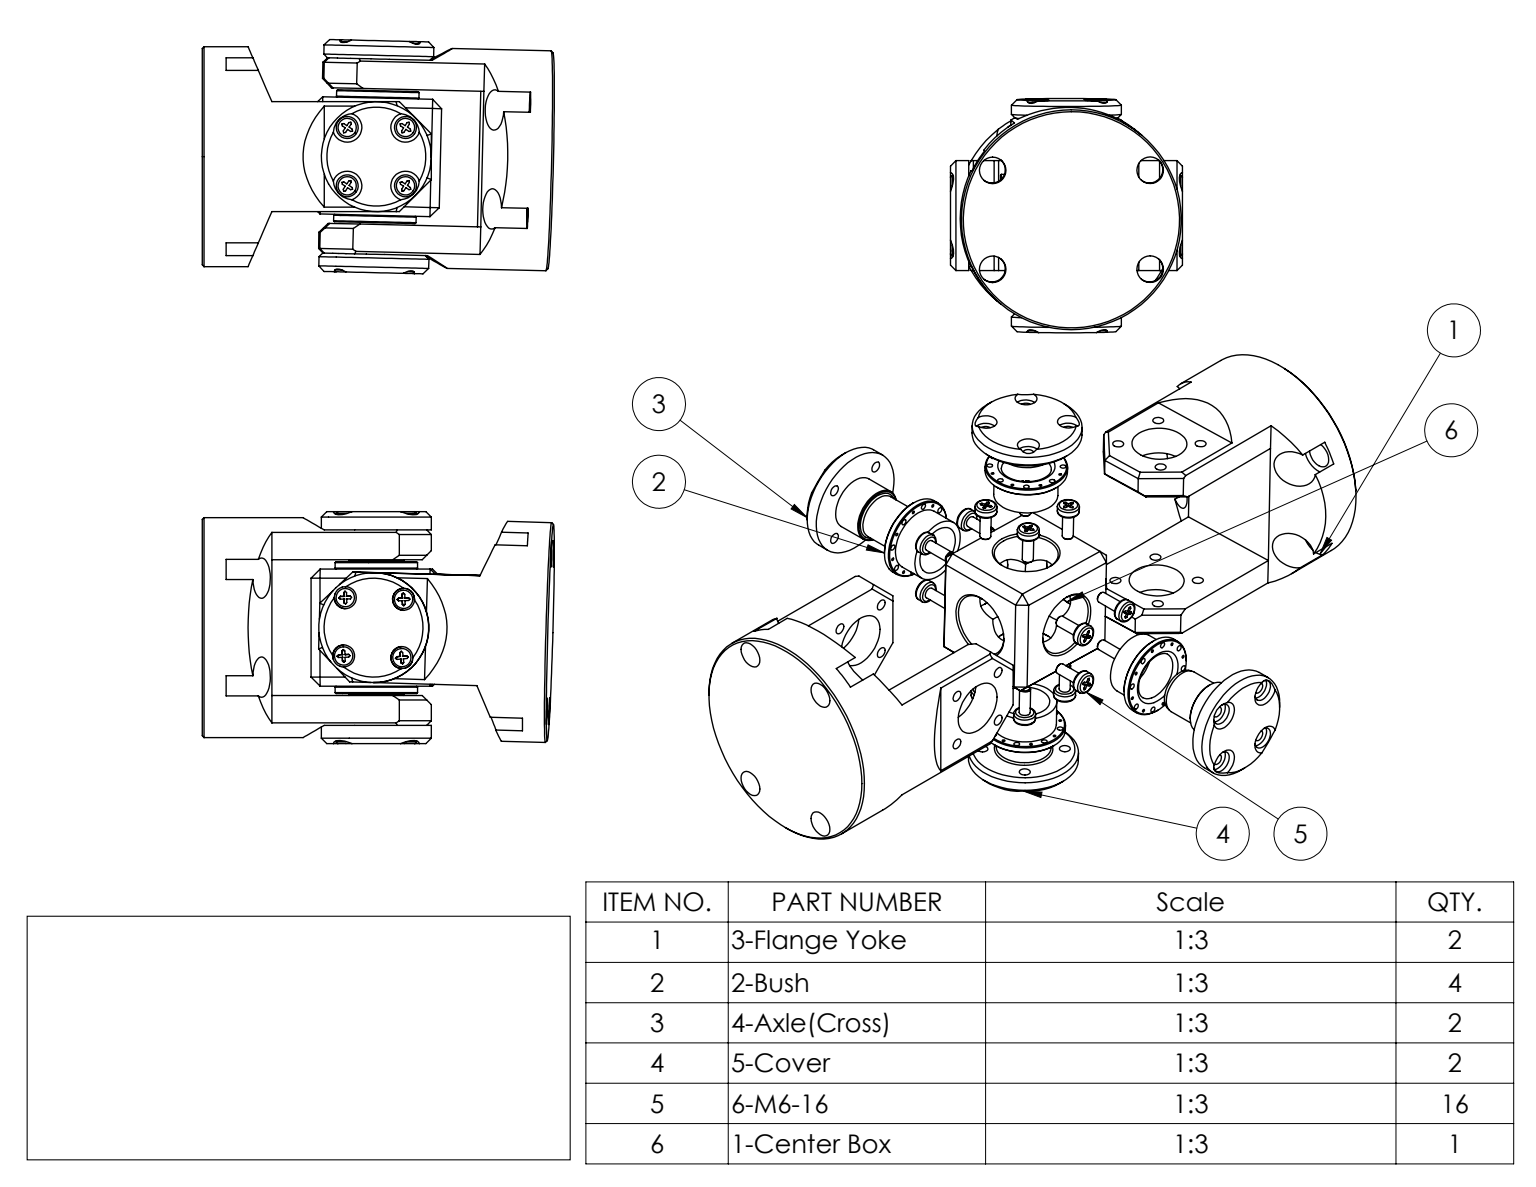
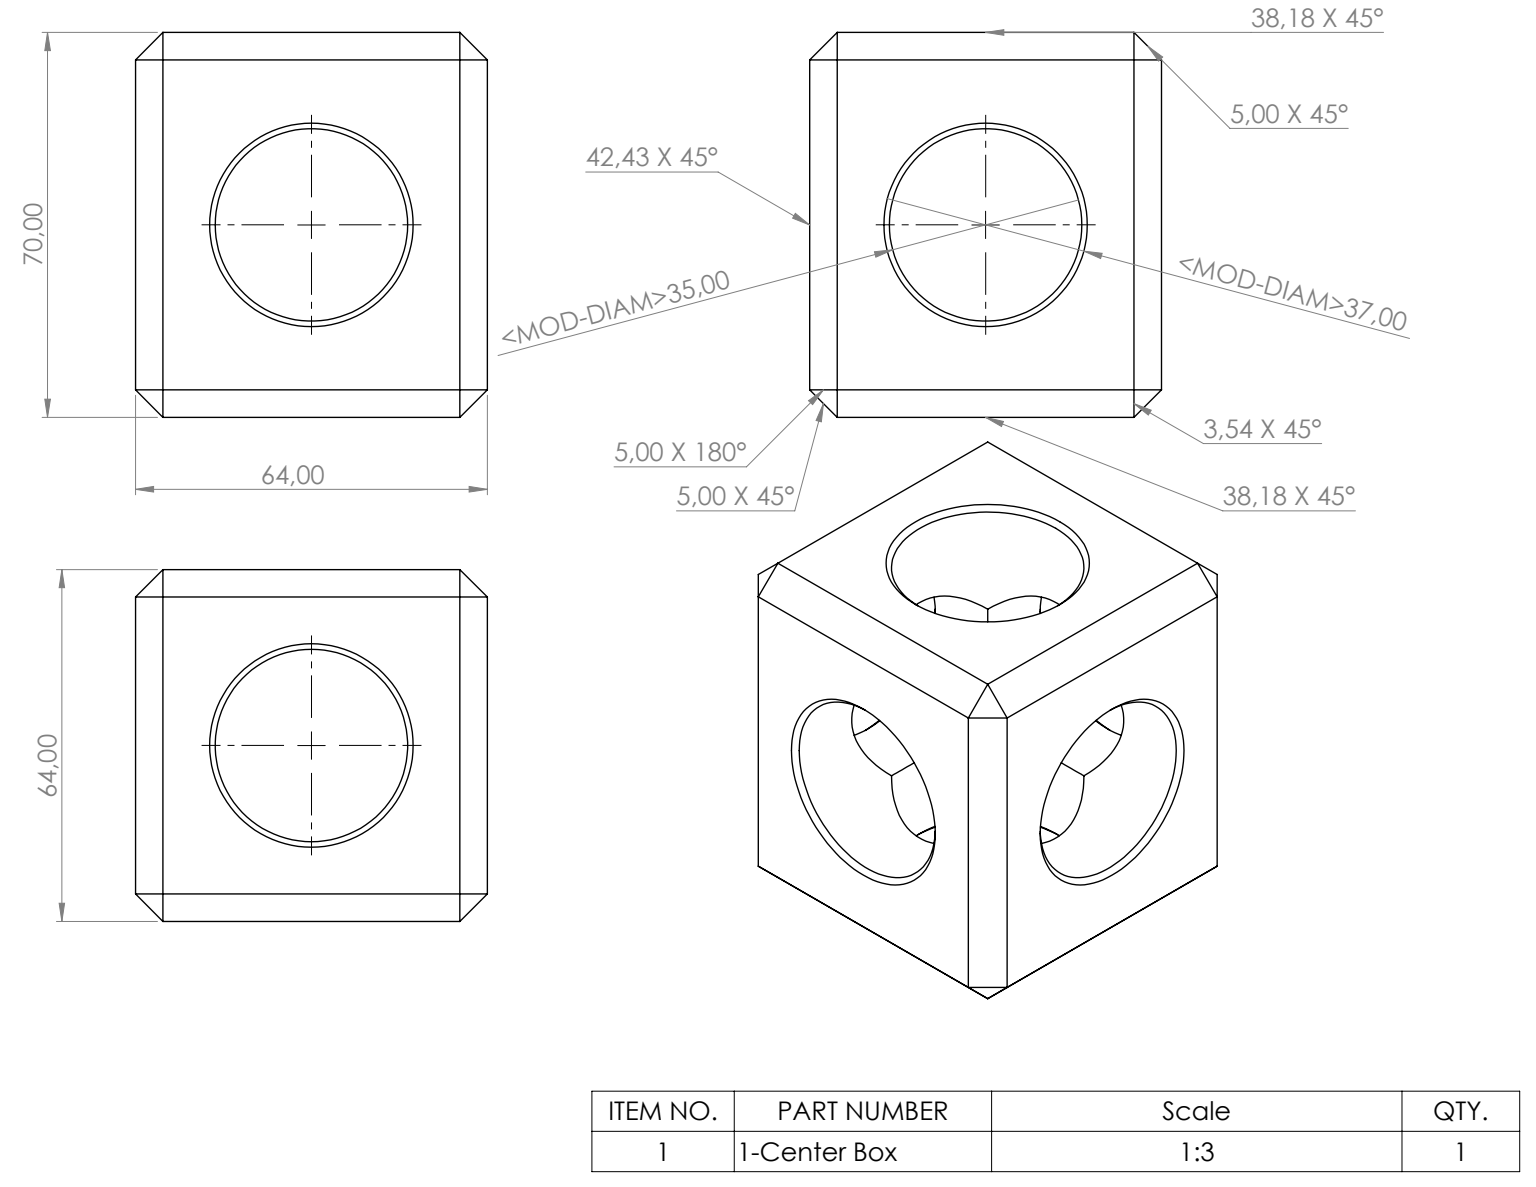
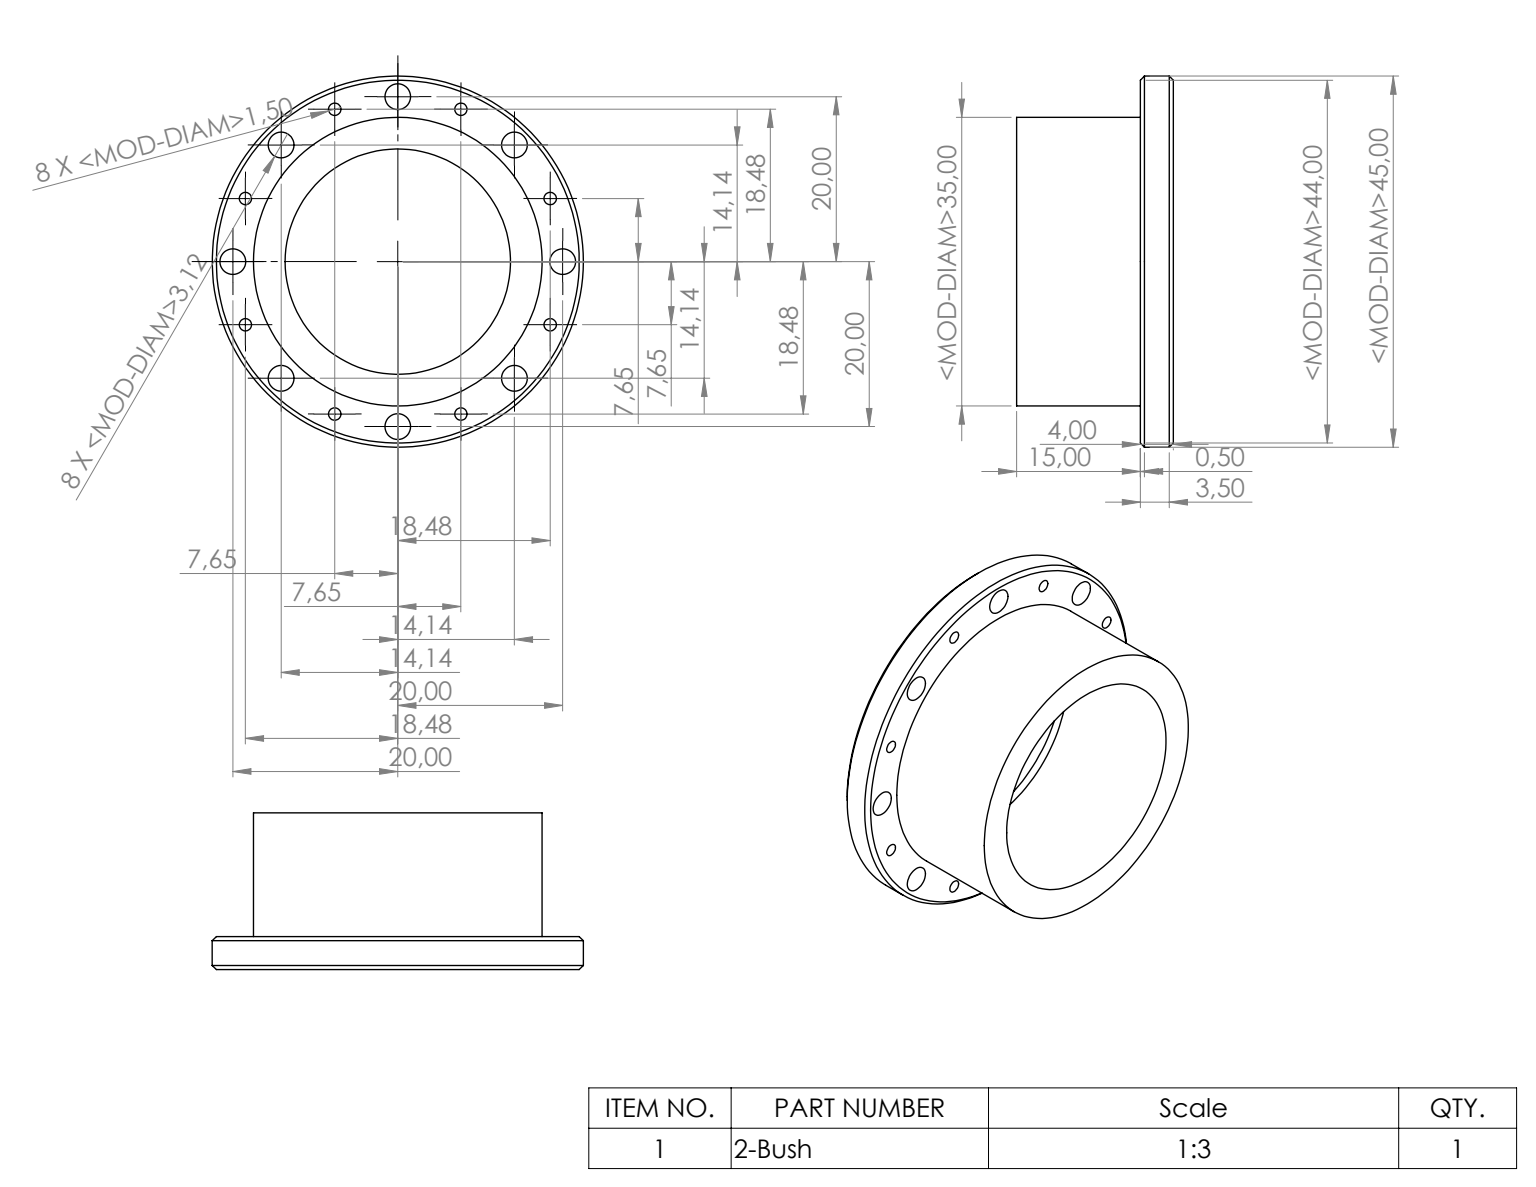
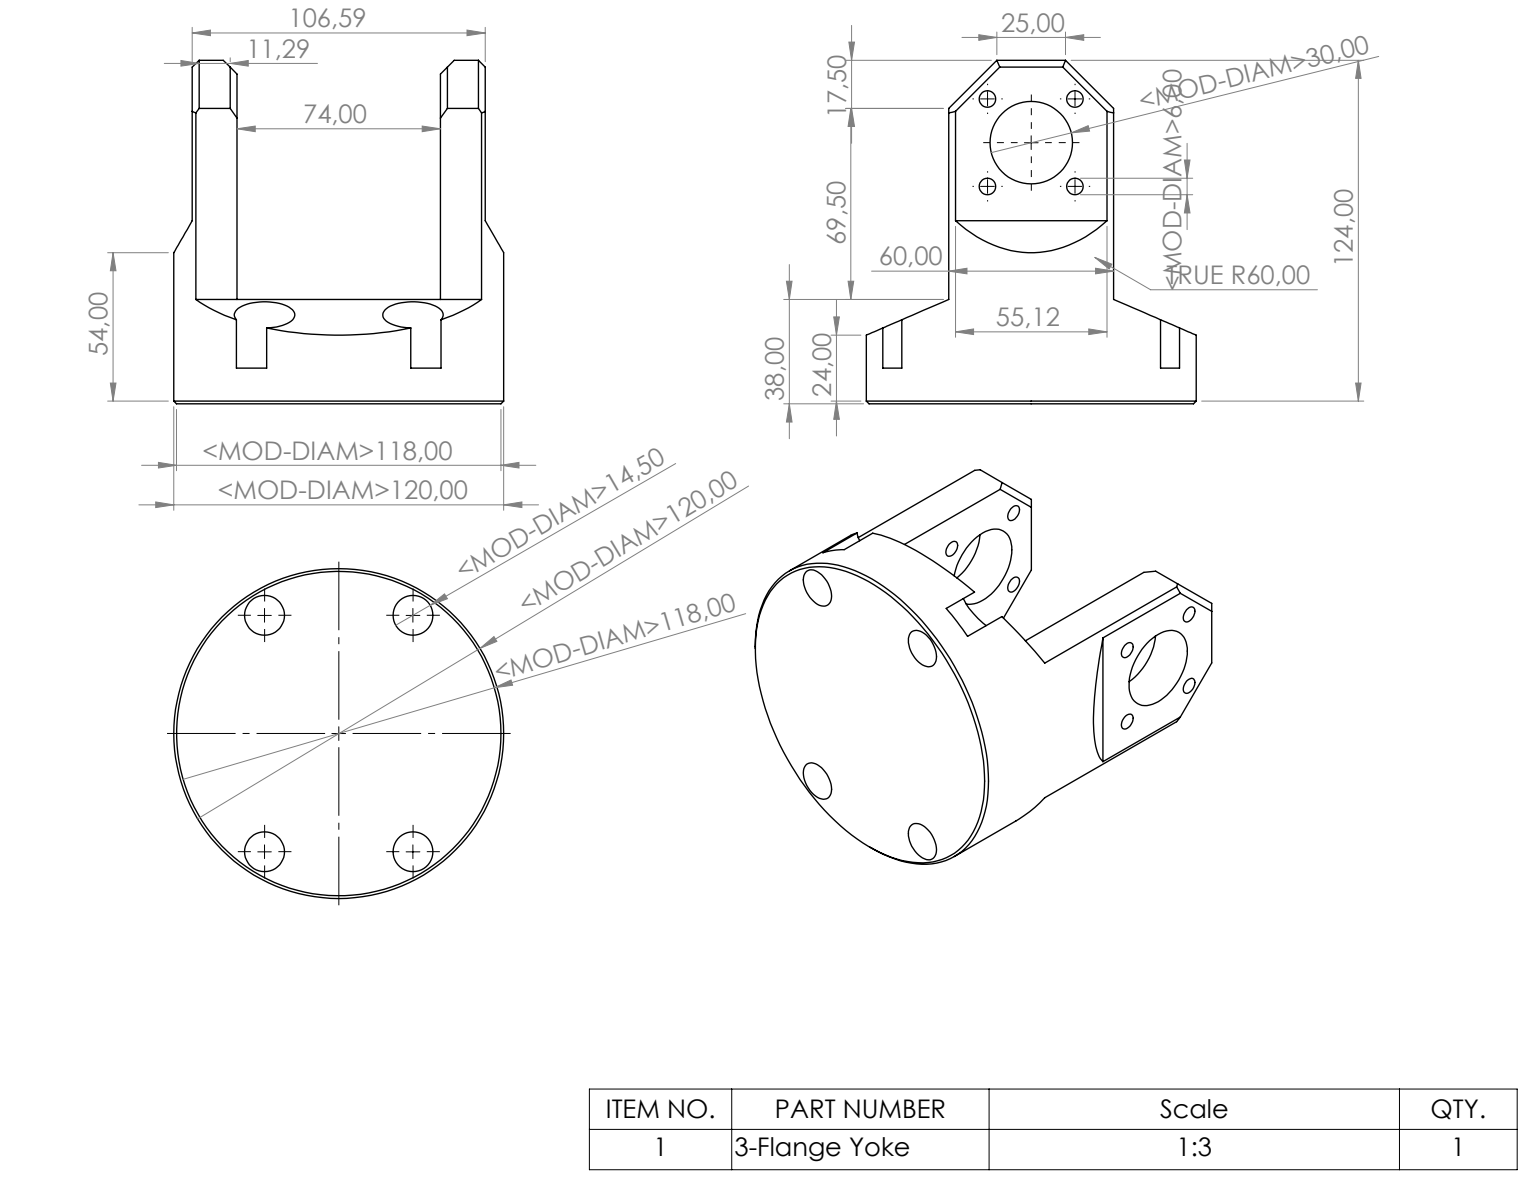
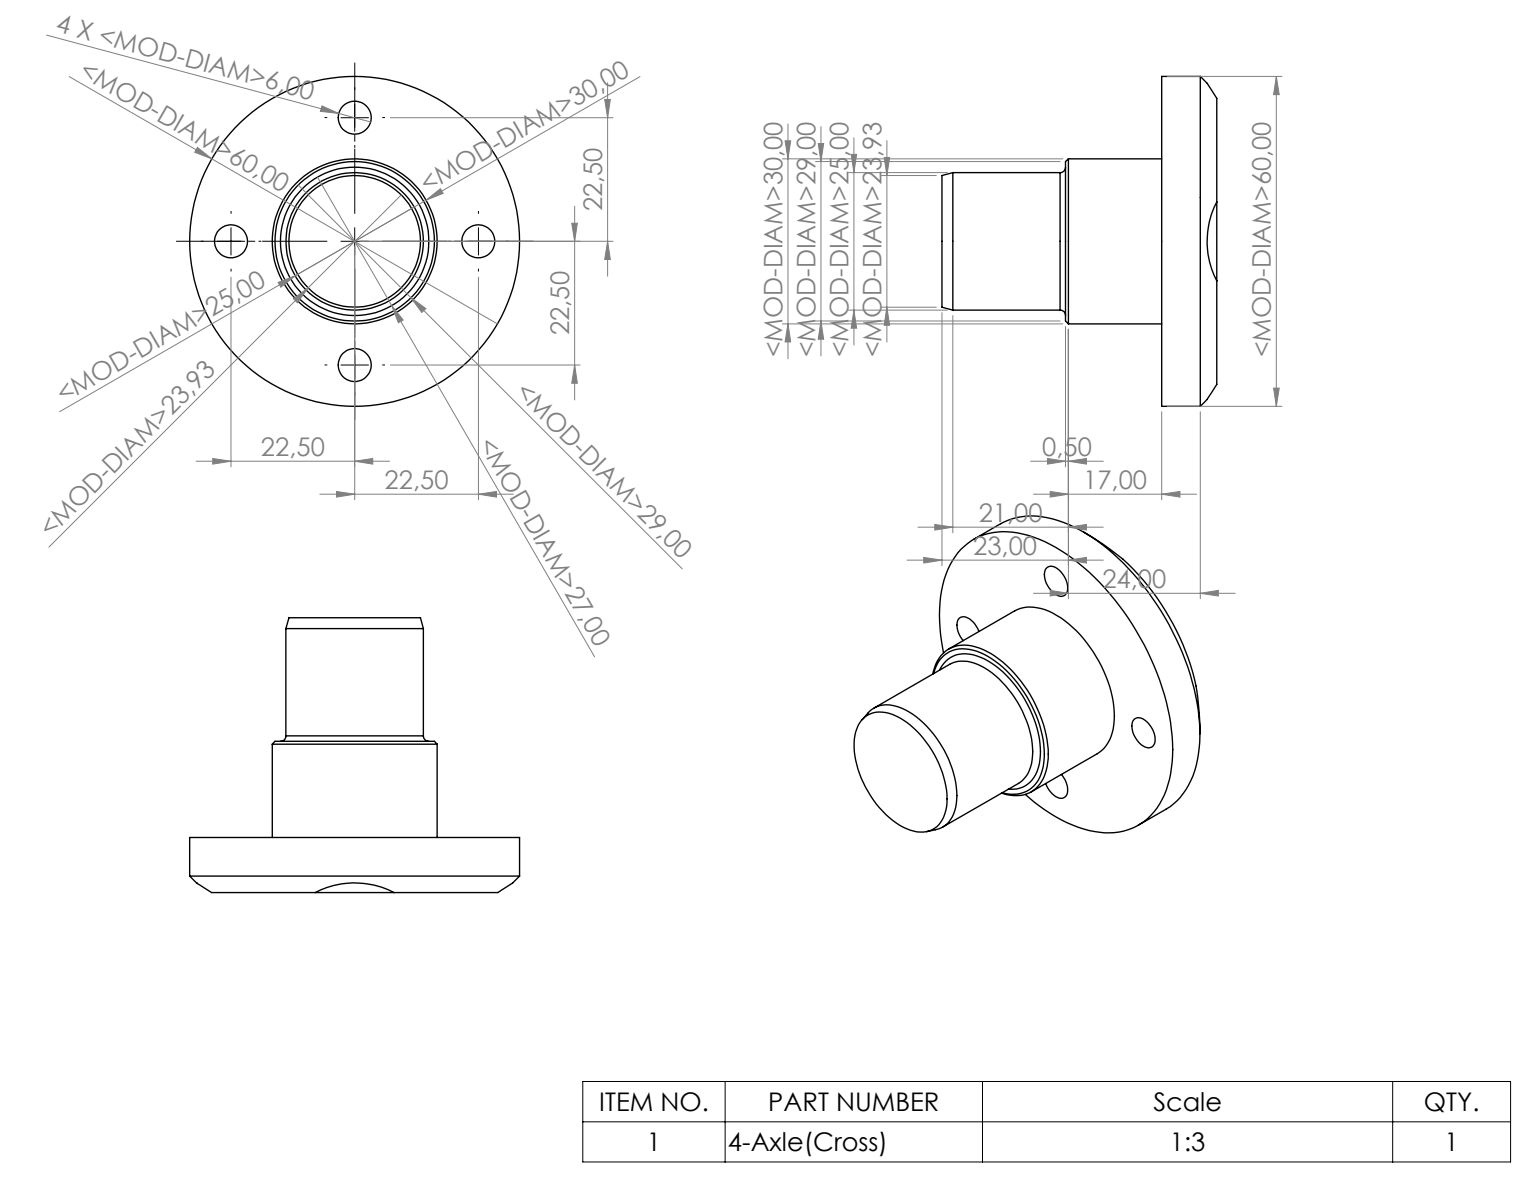
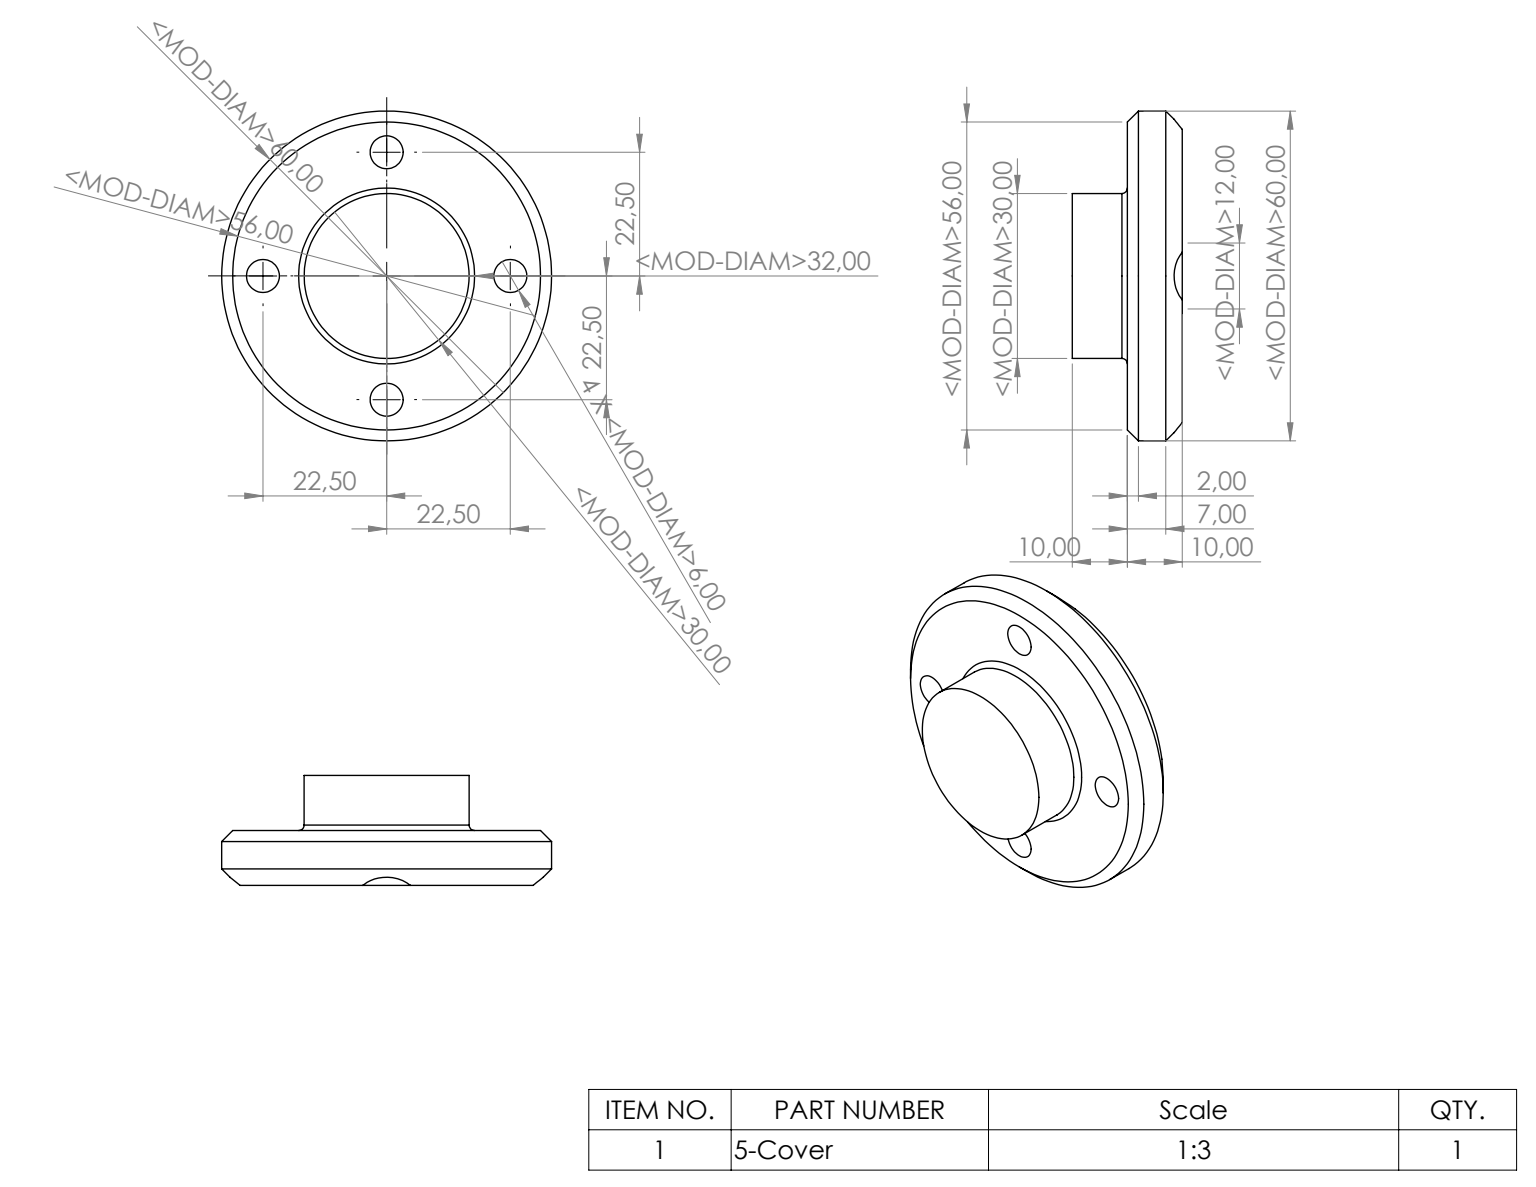
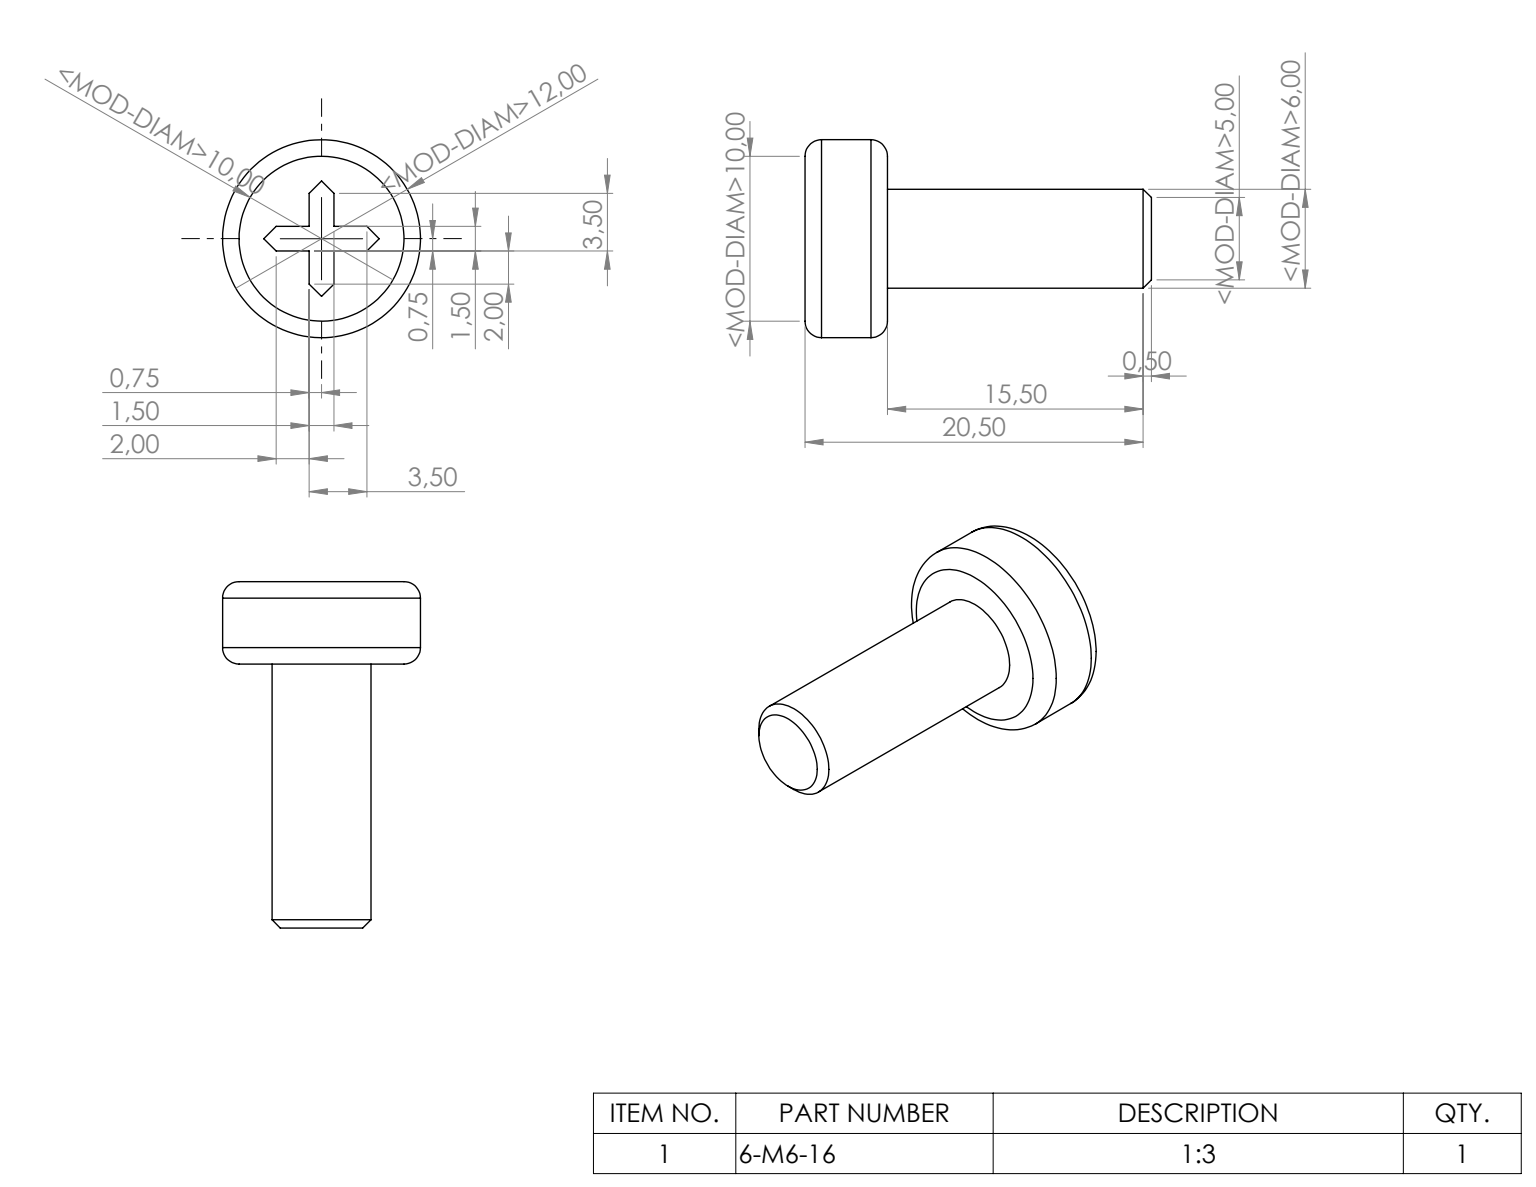
ISO-10303-21;
HEADER;
FILE_DESCRIPTION (('STEP AP214'),
    '1' );
FILE_NAME ('MAT-017',
    '2026-10-28T16:50:19',
    ( '' ),
    ( '' ),
    'SwSTEP 2.0',
    'SolidWorks 2024',
    '' );
FILE_SCHEMA (( 'AUTOMOTIVE_DESIGN' ));
ENDSEC;

DATA;
#1 = DIRECTION ( 'NONE',  ( -0.7071067811865456854, 9.059701919605289623E-16, -0.7071067811865493491 ) ) ;
#2 = FACE_BOUND ( 'NONE', #8236, .T. ) ;
#3 = FACE_OUTER_BOUND ( 'NONE', #2882, .T. ) ;
#4 = ORIENTED_EDGE ( 'NONE', *, *, #2008, .F. ) ;
#5 = EDGE_LOOP ( 'NONE', ( #4798, #3652 ) ) ;
#6 = EDGE_CURVE ( 'NONE', #2372, #8340, #1987, .T. ) ;
#7 = ORIENTED_EDGE ( 'NONE', *, *, #437, .T. ) ;
#8 = DIRECTION ( 'NONE',  ( -2.852901704589927581E-15, -0.02376617340079590149, -0.9997175446104182850 ) ) ;
#9 = ORIENTED_EDGE ( 'NONE', *, *, #306, .F. ) ;
#10 = CARTESIAN_POINT ( 'NONE',  ( -22.50000000000000000, -7.855833012397050680E-14, 5.000000000000000000 ) ) ;
#11 = LINE ( 'NONE', #2843, #879 ) ;
#12 = DIRECTION ( 'NONE',  ( 0.000000000000000000, 0.000000000000000000, -1.000000000000000000 ) ) ;
#13 = CARTESIAN_POINT ( 'NONE',  ( 15.00000000000000000, 1.836970198721029589E-15, 11.00000000000000000 ) ) ;
#14 = CARTESIAN_POINT ( 'NONE',  ( 26.21170834203230982, 53.97171801779368394, -2.612255525622733554 ) ) ;
#15 = EDGE_CURVE ( 'NONE', #5505, #2772, #7117, .T. ) ;
#16 = LINE ( 'NONE', #2270, #110 ) ;
#17 = CIRCLE ( 'NONE', #5073, 3.000000000000000444 ) ;
#18 = VERTEX_POINT ( 'NONE', #6645 ) ;
#19 = EDGE_CURVE ( 'NONE', #8372, #438, #65, .T. ) ;
#20 = DIRECTION ( 'NONE',  ( 0.000000000000000000, 0.000000000000000000, -1.000000000000000000 ) ) ;
#21 = EDGE_CURVE ( 'NONE', #6915, #8464, #3515, .T. ) ;
#22 = EDGE_CURVE ( 'NONE', #2924, #3020, #3177, .T. ) ;
#23 = VERTEX_POINT ( 'NONE', #8844 ) ;
#24 = DIRECTION ( 'NONE',  ( 0.7071067811865494601, 0.7071067811865455743, 0.000000000000000000 ) ) ;
#25 = DIRECTION ( 'NONE',  ( -1.000000000000000000, 0.000000000000000000, 0.000000000000000000 ) ) ;
#26 = VECTOR ( 'NONE', #5373, 1000.000000000000000 ) ;
#27 = LINE ( 'NONE', #8090, #5201 ) ;
#28 = DIRECTION ( 'NONE',  ( -1.000000000000000000, -0.000000000000000000, -0.000000000000000000 ) ) ;
#29 = PRODUCT_DEFINITION_SHAPE ( 'NONE', 'NONE',  #9491 ) ;
#30 = ORIENTED_EDGE ( 'NONE', *, *, #4937, .F. ) ;
#31 = VERTEX_POINT ( 'NONE', #8796 ) ;
#32 = CARTESIAN_POINT ( 'NONE',  ( 3.791949971500756078, 27.16611547376996683, 0.4273392542514659609 ) ) ;
#33 = ORIENTED_EDGE ( 'NONE', *, *, #310, .F. ) ;
#34 = DIRECTION ( 'NONE',  ( 0.000000000000000000, 0.000000000000000000, 1.000000000000000000 ) ) ;
#35 = CARTESIAN_POINT ( 'NONE',  ( 28.50000000000000355, 7.347880794884122694E-16, 5.000000000000000000 ) ) ;
#36 =( BOUNDED_CURVE ( )  B_SPLINE_CURVE ( 3, ( #9430, #2857, #1405, #8718 ),
 .UNSPECIFIED., .F., .F. ) 
 B_SPLINE_CURVE_WITH_KNOTS ( ( 4, 4 ),
 ( 0.6692669939101983934, 1.047197551196597853 ),
 .UNSPECIFIED. ) 
 CURVE ( )  GEOMETRIC_REPRESENTATION_ITEM ( )  RATIONAL_B_SPLINE_CURVE ( ( 1.000000000000000000, 0.9881327504826167285, 0.9881327504826167285, 1.000000000000000000 ) ) 
 REPRESENTATION_ITEM ( '' )  );
#37 = EDGE_CURVE ( 'NONE', #4781, #2523, #3325, .T. ) ;
#38 = CARTESIAN_POINT ( 'NONE',  ( 0.7500000000000000000, 2.749999999999995559, 0.000000000000000000 ) ) ;
#39 = AXIS2_PLACEMENT_3D ( 'NONE', #7750, #9043, #8374 ) ;
#40 = CARTESIAN_POINT ( 'NONE',  ( 29.50000000000000711, -29.99999999999996447, 2.500000000000015543 ) ) ;
#41 = LINE ( 'NONE', #8503, #1449 ) ;
#42 = ADVANCED_FACE ( 'NONE', ( #1448 ), #3565, .F. ) ;
#43 = FACE_OUTER_BOUND ( 'NONE', #6081, .T. ) ;
#44 = CARTESIAN_POINT ( 'NONE',  ( 0.000000000000000000, 0.000000000000000000, 0.000000000000000000 ) ) ;
#45 = ORIENTED_EDGE ( 'NONE', *, *, #8118, .F. ) ;
#46 = ORIENTED_EDGE ( 'NONE', *, *, #483, .F. ) ;
#47 = CARTESIAN_POINT ( 'NONE',  ( -53.29490495164537833, 15.90990257669733943, -54.09009742330271564 ) ) ;
#48 = VECTOR ( 'NONE', #5303, 999.9999999999998863 ) ;
#49 = CARTESIAN_POINT ( 'NONE',  ( 34.25000000000000000, -43.00000000000000000, -25.00000000000000000 ) ) ;
#50 = FACE_OUTER_BOUND ( 'NONE', #5817, .T. ) ;
#51 = DIRECTION ( 'NONE',  ( 0.000000000000000000, 0.000000000000000000, 1.000000000000000000 ) ) ;
#52 = ORIENTED_EDGE ( 'NONE', *, *, #8438, .F. ) ;
#53 = EDGE_LOOP ( 'NONE', ( #8094, #7825 ) ) ;
#54 = CARTESIAN_POINT ( 'NONE',  ( -56.07586385285965491, 64.54333883338065903, 59.86606487507440022 ) ) ;
#55 = VERTEX_POINT ( 'NONE', #1398 ) ;
#56 = EDGE_CURVE ( 'NONE', #523, #4316, #9131, .T. ) ;
#57 = CARTESIAN_POINT ( 'NONE',  ( 29.50000000000000711, -32.49999999999997868, 58.99999999999997158 ) ) ;
#58 = DIRECTION ( 'NONE',  ( -1.000000000000000000, 0.000000000000000000, 0.000000000000000000 ) ) ;
#59 = AXIS2_PLACEMENT_3D ( 'NONE', #1262, #1856, #6375 ) ;
#60 = ADVANCED_FACE ( 'NONE', ( #7941 ), #7013, .F. ) ;
#61 = DIRECTION ( 'NONE',  ( 1.000000000000000000, 0.000000000000000000, 0.000000000000000000 ) ) ;
#62 = CARTESIAN_POINT ( 'NONE',  ( -53.29490495164537833, 15.90990257669733943, -85.90990257669729147 ) ) ;
#63 = CARTESIAN_POINT ( 'NONE',  ( -53.29490495164537833, 15.90990257669733943, -51.09009742330271564 ) ) ;
#64 = EDGE_LOOP ( 'NONE', ( #9455, #3764, #9081, #6496 ) ) ;
#65 = LINE ( 'NONE', #2077, #6706 ) ;
#66 = ORIENTED_EDGE ( 'NONE', *, *, #5730, .F. ) ;
#67 = FACE_OUTER_BOUND ( 'NONE', #9174, .T. ) ;
#68 = CYLINDRICAL_SURFACE ( 'NONE', #4244, 3.000000000000000000 ) ;
#69 = LINE ( 'NONE', #4584, #4436 ) ;
#70 = AXIS2_PLACEMENT_3D ( 'NONE', #3786, #2250, #5184 ) ;
#71 = CARTESIAN_POINT ( 'NONE',  ( 53.29490495164537833, -30.00000000000000000, -97.50000000000002842 ) ) ;
#72 = TOROIDAL_SURFACE ( 'NONE', #5447, 15.66147716702868209, 2.000000000000000000 ) ;
#73 = ORIENTED_EDGE ( 'NONE', *, *, #437, .F. ) ;
#74 = ORIENTED_EDGE ( 'NONE', *, *, #37, .F. ) ;
#75 = VERTEX_POINT ( 'NONE', #1302 ) ;
#76 = FACE_OUTER_BOUND ( 'NONE', #1771, .T. ) ;
#77 = CARTESIAN_POINT ( 'NONE',  ( -4.703319286132082055, 17.49999999999999645, 14.50000000000000178 ) ) ;
#78 = ADVANCED_FACE ( 'NONE', ( #8660 ), #4237, .F. ) ;
#79 = DIRECTION ( 'NONE',  ( 1.000000000000000000, 0.000000000000000000, 0.000000000000000000 ) ) ;
#80 = AXIS2_PLACEMENT_3D ( 'NONE', #2507, #6973, #1060 ) ;
#81 = DIRECTION ( 'NONE',  ( 0.000000000000000000, 0.000000000000000000, -1.000000000000000000 ) ) ;
#82 = DIRECTION ( 'NONE',  ( -1.000000000000000000, 0.000000000000000000, 0.000000000000000000 ) ) ;
#83 = DIRECTION ( 'NONE',  ( 1.224646799147353207E-16, 1.000000000000000000, -0.000000000000000000 ) ) ;
#84 = DIRECTION ( 'NONE',  ( -1.000000000000000000, -0.000000000000000000, -0.000000000000000000 ) ) ;
#85 = VERTEX_POINT ( 'NONE', #733 ) ;
#86 = EDGE_LOOP ( 'NONE', ( #7800, #8743 ) ) ;
#87 = CARTESIAN_POINT ( 'NONE',  ( -19.50000000000000355, 3.673940397442054445E-16, 5.000000000000000000 ) ) ;
#88 = EDGE_LOOP ( 'NONE', ( #1645, #1926, #910, #5468 ) ) ;
#89 = DIRECTION ( 'NONE',  ( 1.000000000000000000, -0.000000000000000000, -0.000000000000000000 ) ) ;
#90 = CARTESIAN_POINT ( 'NONE',  ( 6.702350214711367826, 26.42345776824586423, 0.2543657081580636414 ) ) ;
#91 = DIRECTION ( 'NONE',  ( -0.000000000000000000, -1.000000000000000000, -0.000000000000000000 ) ) ;
#92 = UNCERTAINTY_MEASURE_WITH_UNIT (LENGTH_MEASURE( 1.000000000000000082E-05 ), #7663, 'distance_accuracy_value', 'NONE');
#93 = CARTESIAN_POINT ( 'NONE',  ( 5.000000000000000000, 14.14213562373112154, -14.14213562373077870 ) ) ;
#94 = VECTOR ( 'NONE', #809, 1000.000000000000000 ) ;
#95 = VERTEX_POINT ( 'NONE', #8709 ) ;
#96 = ORIENTED_EDGE ( 'NONE', *, *, #7565, .T. ) ;
#97 = DIRECTION ( 'NONE',  ( 1.000000000000000222, -1.235987831730286119E-16, -8.658028549763971743E-17 ) ) ;
#98 = CARTESIAN_POINT ( 'NONE',  ( 37.00000000000000000, -30.00000000000000000, -95.00000000000000000 ) ) ;
#99 = LINE ( 'NONE', #8746, #418 ) ;
#100 = AXIS2_PLACEMENT_3D ( 'NONE', #6905, #316, #3150 ) ;
#101 = CARTESIAN_POINT ( 'NONE',  ( 0.000000000000000000, 0.000000000000000000, 11.99999999999999645 ) ) ;
#102 = DIRECTION ( 'NONE',  ( -1.000000000000000000, 0.000000000000000000, 0.000000000000000000 ) ) ;
#103 = DIRECTION ( 'NONE',  ( -0.000000000000000000, 0.7071067811865473507, 0.7071067811865477948 ) ) ;
#104 = EDGE_CURVE ( 'NONE', #1161, #4913, #2730, .T. ) ;
#105 = CARTESIAN_POINT ( 'NONE',  ( 4.000000000000000000, 20.00000000000120437, 1.559999999999680531 ) ) ;
#106 = VERTEX_POINT ( 'NONE', #5874 ) ;
#107 = AXIS2_PLACEMENT_3D ( 'NONE', #3229, #1109, #5357 ) ;
#108 = FILL_AREA_STYLE ('',( #7504 ) ) ;
#109 = EDGE_LOOP ( 'NONE', ( #8068, #7356, #2708, #2295 ) ) ;
#110 = VECTOR ( 'NONE', #4520, 1000.000000000000000 ) ;
#111 = CARTESIAN_POINT ( 'NONE',  ( 19.62310601229373930, -19.62310601229373930, 26.87436867076458924 ) ) ;
#112 = EDGE_CURVE ( 'NONE', #6044, #3779, #6462, .T. ) ;
#113 = CARTESIAN_POINT ( 'NONE',  ( 0.000000000000000000, 0.000000000000000000, 0.000000000000000000 ) ) ;
#114 = AXIS2_PLACEMENT_3D ( 'NONE', #1241, #6492, #8505 ) ;
#115 = CIRCLE ( 'NONE', #3792, 1.559999999998939346 ) ;
#116 = CARTESIAN_POINT ( 'NONE',  ( 37.00000000000000000, -15.90990257669733943, -88.90990257669730568 ) ) ;
#117 = AXIS2_PLACEMENT_3D ( 'NONE', #9182, #529, #8560 ) ;
#118 = CARTESIAN_POINT ( 'NONE',  ( -28.50000000000000355, 0.000000000000000000, 5.000000000000000000 ) ) ;
#119 = VECTOR ( 'NONE', #1429, 1000.000000000000114 ) ;
#120 = ORIENTED_EDGE ( 'NONE', *, *, #516, .T. ) ;
#121 = EDGE_LOOP ( 'NONE', ( #3677, #5526, #8764, #3879, #8157 ) ) ;
#122 = AXIS2_PLACEMENT_3D ( 'NONE', #7775, #7822, #1915 ) ;
#123 = ORIENTED_EDGE ( 'NONE', *, *, #4714, .F. ) ;
#124 = ORIENTED_EDGE ( 'NONE', *, *, #9169, .F. ) ;
#125 = ADVANCED_FACE ( 'NONE', ( #5828 ), #4338, .F. ) ;
#126 = AXIS2_PLACEMENT_3D ( 'NONE', #8460, #4038, #6303 ) ;
#127 = CARTESIAN_POINT ( 'NONE',  ( 37.00000000000000000, 30.00000000000000000, -78.96446609406729067 ) ) ;
#128 = DIRECTION ( 'NONE',  ( 0.000000000000000000, 0.000000000000000000, 1.000000000000000000 ) ) ;
#129 = CYLINDRICAL_SURFACE ( 'NONE', #8083, 3.000000000000000000 ) ;
#130 = AXIS2_PLACEMENT_3D ( 'NONE', #2864, #5798, #1268 ) ;
#131 = CARTESIAN_POINT ( 'NONE',  ( 27.00000000000000355, -29.99999999999999289, 64.00000000000000000 ) ) ;
#132 = DIRECTION ( 'NONE',  ( 1.000000000000000000, 0.000000000000000000, 0.000000000000000000 ) ) ;
#133 = DIRECTION ( 'NONE',  ( 1.000000000000000000, 0.000000000000000000, 0.000000000000000000 ) ) ;
#134 = CYLINDRICAL_SURFACE ( 'NONE', #6817, 11.00000000000000000 ) ;
#135 = EDGE_CURVE ( 'NONE', #3234, #301, #2169, .T. ) ;
#136 = ORIENTED_EDGE ( 'NONE', *, *, #6818, .T. ) ;
#137 = EDGE_CURVE ( 'NONE', #7845, #1132, #8358, .T. ) ;
#138 = ORIENTED_EDGE ( 'NONE', *, *, #426, .F. ) ;
#139 = VECTOR ( 'NONE', #696, 1000.000000000000000 ) ;
#140 = VECTOR ( 'NONE', #6903, 1000.000000000000000 ) ;
#141 = ADVANCED_FACE ( 'NONE', ( #2217 ), #5149, .T. ) ;
#142 = CARTESIAN_POINT ( 'NONE',  ( 2.000000000000000000, 0.000000000000000000, 0.000000000000000000 ) ) ;
#143 = CIRCLE ( 'NONE', #3070, 1.559999999999098552 ) ;
#144 = EDGE_CURVE ( 'NONE', #410, #1266, #6863, .T. ) ;
#145 = EDGE_CURVE ( 'NONE', #5577, #3040, #1032, .T. ) ;
#146 = ORIENTED_EDGE ( 'NONE', *, *, #4940, .T. ) ;
#147 = LINE ( 'NONE', #8971, #1968 ) ;
#148 = VECTOR ( 'NONE', #6018, 1000.000000000000114 ) ;
#149 = FACE_BOUND ( 'NONE', #7075, .T. ) ;
#150 = DIRECTION ( 'NONE',  ( 0.7071067811865441310, -0.7071067811865510144, -0.000000000000000000 ) ) ;
#151 = EDGE_LOOP ( 'NONE', ( #1174, #5770 ) ) ;
#152 = VERTEX_POINT ( 'NONE', #8316 ) ;
#153 = EDGE_CURVE ( 'NONE', #2399, #367, #4869, .T. ) ;
#154 = EDGE_CURVE ( 'NONE', #8069, #2437, #9010, .T. ) ;
#155 = DIRECTION ( 'NONE',  ( 0.000000000000000000, 0.000000000000000000, -1.000000000000000000 ) ) ;
#156 = EDGE_CURVE ( 'NONE', #7922, #4540, #818, .T. ) ;
#157 = DIRECTION ( 'NONE',  ( 0.7071067811865456854, -0.7071067811865493491, 0.000000000000000000 ) ) ;
#158 = DIRECTION ( 'NONE',  ( 0.000000000000000000, 0.000000000000000000, -1.000000000000000000 ) ) ;
#159 = CARTESIAN_POINT ( 'NONE',  ( 0.000000000000000000, -18.47759065022712832, 6.903668647304566974 ) ) ;
#160 = CARTESIAN_POINT ( 'NONE',  ( 53.29490495164537833, 18.67545040036925386, -90.28901569369799063 ) ) ;
#161 = CARTESIAN_POINT ( 'NONE',  ( 4.703319286132084720, 17.49999999999999645, 14.50000000000000178 ) ) ;
#162 = AXIS2_PLACEMENT_3D ( 'NONE', #9418, #584, #3511 ) ;
#163 = PLANE ( 'NONE',  #7256 ) ;
#164 = ORIENTED_EDGE ( 'NONE', *, *, #7741, .T. ) ;
#165 = CARTESIAN_POINT ( 'NONE',  ( 3.499999999999999556, 0.000000000000000000, 0.000000000000000000 ) ) ;
#166 = ORIENTED_EDGE ( 'NONE', *, *, #8588, .F. ) ;
#167 = DIRECTION ( 'NONE',  ( 0.000000000000000000, 0.000000000000000000, 1.000000000000000000 ) ) ;
#168 = CARTESIAN_POINT ( 'NONE',  ( 0.000000000000000000, -14.14213562373112154, 15.70213562373564820 ) ) ;
#169 = DIRECTION ( 'NONE',  ( -1.000000000000000000, 0.000000000000000000, 0.000000000000000000 ) ) ;
#170 = ORIENTED_EDGE ( 'NONE', *, *, #7706, .F. ) ;
#171 = MANIFOLD_SOLID_BREP ( 'Pah2', #1325 ) ;
#172 = ORIENTED_EDGE ( 'NONE', *, *, #9280, .F. ) ;
#173 = ORIENTED_EDGE ( 'NONE', *, *, #8062, .T. ) ;
#174 = ORIENTED_EDGE ( 'NONE', *, *, #2719, .T. ) ;
#175 = CARTESIAN_POINT ( 'NONE',  ( -37.22467645238199196, 47.05659850664387278, 11.99999999999999645 ) ) ;
#176 = DIRECTION ( 'NONE',  ( 0.000000000000000000, -0.000000000000000000, 1.000000000000000000 ) ) ;
#177 = AXIS2_PLACEMENT_3D ( 'NONE', #643, #6371, #687 ) ;
#178 = LINE ( 'NONE', #891, #3319 ) ;
#179 = DIRECTION ( 'NONE',  ( -1.000000000000000000, 0.000000000000000000, 0.000000000000000000 ) ) ;
#180 = CARTESIAN_POINT ( 'NONE',  ( 4.000000000000000000, -14.14213562373248401, -14.14213562372942157 ) ) ;
#181 = SURFACE_STYLE_USAGE ( .BOTH. , #898 ) ;
#182 = DIRECTION ( 'NONE',  ( 0.000000000000000000, 0.000000000000000000, 1.000000000000000000 ) ) ;
#183 = EDGE_LOOP ( 'NONE', ( #6953, #2067, #7066, #3737 ) ) ;
#184 = EDGE_LOOP ( 'NONE', ( #3377, #2801, #2753, #2032 ) ) ;
#185 = CYLINDRICAL_SURFACE ( 'NONE', #862, 3.000000000000000000 ) ;
#186 = ORIENTED_EDGE ( 'NONE', *, *, #3069, .F. ) ;
#187 = DIRECTION ( 'NONE',  ( -1.000000000000000000, 0.000000000000000000, 0.000000000000000000 ) ) ;
#188 = EDGE_LOOP ( 'NONE', ( #6810, #8765 ) ) ;
#189 = AXIS2_PLACEMENT_3D ( 'NONE', #307, #3232, #6985 ) ;
#190 = MANIFOLD_SOLID_BREP ( 'Radyus1', #2569 ) ;
#191 = DIRECTION ( 'NONE',  ( 0.000000000000000000, 1.000000000000000000, 0.000000000000000000 ) ) ;
#192 = EDGE_CURVE ( 'NONE', #9088, #5210, #6690, .T. ) ;
#193 = CYLINDRICAL_SURFACE ( 'NONE', #1753, 0.7499999999989250821 ) ;
#194 = EDGE_CURVE ( 'NONE', #5380, #7603, #3025, .T. ) ;
#195 = UNCERTAINTY_MEASURE_WITH_UNIT (LENGTH_MEASURE( 1.000000000000000082E-05 ), #6680, 'distance_accuracy_value', 'NONE');
#196 = AXIS2_PLACEMENT_3D ( 'NONE', #1778, #5349, #383 ) ;
#197 = EDGE_LOOP ( 'NONE', ( #6623, #3215, #8581, #5552 ) ) ;
#198 = ORIENTED_EDGE ( 'NONE', *, *, #3586, .T. ) ;
#199 = DIRECTION ( 'NONE',  ( 1.544988095791843818E-17, -0.9997175446104179519, 0.02376617340079473228 ) ) ;
#200 = AXIS2_PLACEMENT_3D ( 'NONE', #8510, #1928, #3508 ) ;
#201 = FACE_BOUND ( 'NONE', #3357, .T. ) ;
#202 = CARTESIAN_POINT ( 'NONE',  ( 0.000000000000000000, 2.755455298081544778E-15, -22.50000000000000000 ) ) ;
#203 = APPLICATION_CONTEXT ( 'automotive_design' ) ;
#204 = DIRECTION ( 'NONE',  ( 0.000000000000000000, 0.000000000000000000, 1.000000000000000000 ) ) ;
#205 = CARTESIAN_POINT ( 'NONE',  ( 0.000000000000000000, 0.000000000000000000, 21.00000000000000000 ) ) ;
#206 = CIRCLE ( 'NONE', #2661, 6.000000000000000000 ) ;
#207 = DIRECTION ( 'NONE',  ( 0.000000000000000000, 0.000000000000000000, 1.000000000000000000 ) ) ;
#208 = DIRECTION ( 'NONE',  ( 1.000000000000000000, 0.000000000000000000, 0.000000000000000000 ) ) ;
#209 = ORIENTED_EDGE ( 'NONE', *, *, #5661, .T. ) ;
#210 =( NAMED_UNIT ( * ) PLANE_ANGLE_UNIT ( ) SI_UNIT ( $, .RADIAN. ) );
#211 = EDGE_LOOP ( 'NONE', ( #5742, #6073, #5276, #6526 ) ) ;
#212 = DIRECTION ( 'NONE',  ( -0.000000000000000000, -0.000000000000000000, -1.000000000000000000 ) ) ;
#213 = CARTESIAN_POINT ( 'NONE',  ( -26.99999999999998934, 0.000000000000000000, 64.00000000000000000 ) ) ;
#214 = CIRCLE ( 'NONE', #1119, 2.999999999999999112 ) ;
#215 = PLANE ( 'NONE',  #7192 ) ;
#216 = ORIENTED_EDGE ( 'NONE', *, *, #5023, .T. ) ;
#217 = ORIENTED_EDGE ( 'NONE', *, *, #4535, .F. ) ;
#218 = AXIS2_PLACEMENT_3D ( 'NONE', #4359, #9398, #2914 ) ;
#219 = ORIENTED_EDGE ( 'NONE', *, *, #9105, .T. ) ;
#220 = ORIENTED_EDGE ( 'NONE', *, *, #19, .T. ) ;
#221 = CARTESIAN_POINT ( 'NONE',  ( -17.50000000000000355, 2.143131898507868643E-15, 0.000000000000000000 ) ) ;
#222 = CARTESIAN_POINT ( 'NONE',  ( 38.00000000000000000, -43.00000000000000000, -7.366666666666667140 ) ) ;
#223 = CARTESIAN_POINT ( 'NONE',  ( 28.00000000000000711, 3.551475717527324030E-15, 10.00000000000000000 ) ) ;
#224 = AXIS2_PLACEMENT_3D ( 'NONE', #4931, #4210, #2686 ) ;
#225 = CARTESIAN_POINT ( 'NONE',  ( -53.29490495164537833, -3.673940397442057600E-15, -70.00000000000000000 ) ) ;
#226 = CARTESIAN_POINT ( 'NONE',  ( 13.50000000000000178, 0.000000000000000000, 27.50000000000000355 ) ) ;
#227 = CARTESIAN_POINT ( 'NONE',  ( -22.50000000000000000, -7.855833012397050680E-14, 10.00000000000000000 ) ) ;
#228 = EDGE_CURVE ( 'NONE', #3453, #8277, #1798, .T. ) ;
#229 = ORIENTED_EDGE ( 'NONE', *, *, #269, .F. ) ;
#230 = MECHANICAL_DESIGN_GEOMETRIC_PRESENTATION_REPRESENTATION (  '', ( #5131 ), #1330 ) ;
#231 = EDGE_LOOP ( 'NONE', ( #8033, #1343, #3899, #2281 ) ) ;
#232 = CARTESIAN_POINT ( 'NONE',  ( -60.00000000000000000, -30.00000000000000000, -30.00000000000000000 ) ) ;
#233 = VERTEX_POINT ( 'NONE', #4579 ) ;
#234 = CARTESIAN_POINT ( 'NONE',  ( -38.00000000000000711, -43.00000000000000000, 11.99999999999999645 ) ) ;
#235 = DIRECTION ( 'NONE',  ( 0.7071067811865456854, -0.7071067811865493491, -0.000000000000000000 ) ) ;
#236 = CONICAL_SURFACE ( 'NONE', #4063, 14.49999999999998401, 0.7853981633974533860 ) ;
#237 = ORIENTED_EDGE ( 'NONE', *, *, #1949, .T. ) ;
#238 = ADVANCED_FACE ( 'NONE', ( #2419 ), #1693, .F. ) ;
#239 = CARTESIAN_POINT ( 'NONE',  ( 0.000000000000000000, 0.000000000000000000, 0.000000000000000000 ) ) ;
#240 = CARTESIAN_POINT ( 'NONE',  ( 37.00000000000000000, -30.00000000000000000, -95.00000000000000000 ) ) ;
#241 = DIRECTION ( 'NONE',  ( 1.000000000000000000, 0.000000000000000000, 0.000000000000000000 ) ) ;
#242 = EDGE_LOOP ( 'NONE', ( #3695, #2216, #389, #7076 ) ) ;
#243 = ORIENTED_EDGE ( 'NONE', *, *, #7351, .F. ) ;
#244 = PRODUCT_CONTEXT ( 'NONE', #4133, 'mechanical' ) ;
#245 = FACE_OUTER_BOUND ( 'NONE', #280, .T. ) ;
#246 = CARTESIAN_POINT ( 'NONE',  ( 4.000000000000000000, -7.653668647303860872, -19.22759065022669134 ) ) ;
#247 = DIRECTION ( 'NONE',  ( 0.000000000000000000, 0.000000000000000000, -1.000000000000000000 ) ) ;
#248 = AXIS2_PLACEMENT_3D ( 'NONE', #8435, #4780, #4912 ) ;
#249 = LINE ( 'NONE', #1829, #3671 ) ;
#250 = PRODUCT_RELATED_PRODUCT_CATEGORY ( 'part', '', ( #4471 ) ) ;
#251 = EDGE_CURVE ( 'NONE', #900, #5694, #9127, .T. ) ;
#252 = DIRECTION ( 'NONE',  ( 0.000000000000000000, 0.000000000000000000, -1.000000000000000000 ) ) ;
#253 = ADVANCED_FACE ( 'NONE', ( #9175 ), #2610, .T. ) ;
#254 = EDGE_LOOP ( 'NONE', ( #5839, #6022, #2019, #3735 ) ) ;
#255 = ADVANCED_FACE ( 'NONE', ( #7915 ), #7696, .F. ) ;
#256 = ORIENTED_EDGE ( 'NONE', *, *, #3726, .F. ) ;
#257 = DIRECTION ( 'NONE',  ( -1.000000000000000000, 0.000000000000000000, 0.000000000000000000 ) ) ;
#258 = EDGE_CURVE ( 'NONE', #4079, #5088, #663, .T. ) ;
#259 = LINE ( 'NONE', #9083, #2418 ) ;
#260 = CARTESIAN_POINT ( 'NONE',  ( 60.00000000000000000, -30.00000000000000355, -82.50000000000001421 ) ) ;
#261 = CARTESIAN_POINT ( 'NONE',  ( -37.00000000000000711, -15.90990257669733943, -88.90990257669730568 ) ) ;
#262 = VECTOR ( 'NONE', #7846, 1000.000000000000000 ) ;
#263 = VECTOR ( 'NONE', #2002, 1000.000000000000000 ) ;
#264 = ORIENTED_EDGE ( 'NONE', *, *, #9231, .T. ) ;
#265 = ORIENTED_EDGE ( 'NONE', *, *, #8257, .F. ) ;
#266 = EDGE_LOOP ( 'NONE', ( #1164, #7378, #7869, #3274 ) ) ;
#267 = ORIENTED_EDGE ( 'NONE', *, *, #4163, .F. ) ;
#268 = DIRECTION ( 'NONE',  ( 0.000000000000000000, 0.000000000000000000, 1.000000000000000000 ) ) ;
#269 = EDGE_CURVE ( 'NONE', #6362, #5838, #4273, .T. ) ;
#270 = CARTESIAN_POINT ( 'NONE',  ( -17.50000000000000355, 2.143131898507868643E-15, 49.50000000000000000 ) ) ;
#271 = CARTESIAN_POINT ( 'NONE',  ( 0.000000000000000000, 34.00000000000001421, 32.00000000000000000 ) ) ;
#272 = DIRECTION ( 'NONE',  ( 0.000000000000000000, 0.000000000000000000, 1.000000000000000000 ) ) ;
#273 = AXIS2_PLACEMENT_3D ( 'NONE', #2075, #1350, #8564 ) ;
#274 = DIRECTION ( 'NONE',  ( -0.7071067811865454633, 0.000000000000000000, -0.7071067811865494601 ) ) ;
#275 = VECTOR ( 'NONE', #434, 1000.000000000000000 ) ;
#276 = DIRECTION ( 'NONE',  ( -1.000000000000000000, -0.000000000000000000, -0.000000000000000000 ) ) ;
#277 = VECTOR ( 'NONE', #4768, 1000.000000000000000 ) ;
#278 = DIRECTION ( 'NONE',  ( -1.000000000000000000, 0.000000000000000000, 0.000000000000000000 ) ) ;
#279 = CIRCLE ( 'NONE', #8252, 11.00000000000000711 ) ;
#280 = EDGE_LOOP ( 'NONE', ( #6235, #8043, #8671, #1683 ) ) ;
#281 = ORIENTED_EDGE ( 'NONE', *, *, #5945, .F. ) ;
#282 = PLANE ( 'NONE',  #9433 ) ;
#283 = ORIENTED_EDGE ( 'NONE', *, *, #3869, .F. ) ;
#284 = LINE ( 'NONE', #8259, #4546 ) ;
#285 = DIRECTION ( 'NONE',  ( 0.000000000000000000, 0.000000000000000000, -1.000000000000000000 ) ) ;
#286 = AXIS2_PLACEMENT_3D ( 'NONE', #6476, #7052, #8583 ) ;
#287 = VERTEX_POINT ( 'NONE', #5444 ) ;
#288 = DIRECTION ( 'NONE',  ( 0.000000000000000000, 0.000000000000000000, -1.000000000000000000 ) ) ;
#289 = AXIS2_PLACEMENT_3D ( 'NONE', #5072, #4352, #128 ) ;
#290 = CARTESIAN_POINT ( 'NONE',  ( 37.00000000000000000, -15.90990257669733943, -85.90990257669729147 ) ) ;
#291 = CARTESIAN_POINT ( 'NONE',  ( 5.103771271004210242, -27.45068023253072909, 0.9147230066269097515 ) ) ;
#292 = EDGE_LOOP ( 'NONE', ( #1795, #5038, #1091, #7202 ) ) ;
#293 = ORIENTED_EDGE ( 'NONE', *, *, #3069, .T. ) ;
#294 = PRODUCT_CONTEXT ( 'NONE', #1478, 'mechanical' ) ;
#295 = VECTOR ( 'NONE', #2775, 1000.000000000000000 ) ;
#296 = FACE_OUTER_BOUND ( 'NONE', #7526, .T. ) ;
#297 = CARTESIAN_POINT ( 'NONE',  ( 12.37436867076458036, 12.37436867076458036, 44.37436867076458213 ) ) ;
#298 = CARTESIAN_POINT ( 'NONE',  ( 0.000000000000000000, 9.603694566548697359E-13, 20.00000000000290612 ) ) ;
#299 = FACE_OUTER_BOUND ( 'NONE', #231, .T. ) ;
#300 = CARTESIAN_POINT ( 'NONE',  ( -26.42320443315921352, 6.702656137449878315, 0.2542028498880767873 ) ) ;
#301 = VERTEX_POINT ( 'NONE', #6269 ) ;
#302 = EDGE_LOOP ( 'NONE', ( #8368, #9024 ) ) ;
#303 = CARTESIAN_POINT ( 'NONE',  ( 0.000000000000000000, -30.00000000000000000, 0.000000000000000000 ) ) ;
#304 = DIRECTION ( 'NONE',  ( -1.000000000000000000, -0.000000000000000000, -0.000000000000000000 ) ) ;
#305 = LINE ( 'NONE', #9085, #4587 ) ;
#306 = EDGE_CURVE ( 'NONE', #1076, #8284, #1106, .T. ) ;
#307 = CARTESIAN_POINT ( 'NONE',  ( 5.000000000000000000, 14.14213562373112154, -14.14213562373077870 ) ) ;
#308 = EDGE_CURVE ( 'NONE', #4536, #5331, #8465, .T. ) ;
#309 = ORIENTED_EDGE ( 'NONE', *, *, #4551, .T. ) ;
#310 = EDGE_CURVE ( 'NONE', #883, #5200, #6979, .T. ) ;
#311 = ADVANCED_FACE ( 'NONE', ( #7870 ), #616, .F. ) ;
#312 = ORIENTED_EDGE ( 'NONE', *, *, #829, .F. ) ;
#313 = VERTEX_POINT ( 'NONE', #3493 ) ;
#314 = CARTESIAN_POINT ( 'NONE',  ( -53.29490495164537833, -27.56180520566615044, -81.40266088840114378 ) ) ;
#315 = DIRECTION ( 'NONE',  ( 1.000000000000000000, 0.000000000000000000, 0.000000000000000000 ) ) ;
#316 = DIRECTION ( 'NONE',  ( -1.000000000000000000, 0.000000000000000000, 0.000000000000000000 ) ) ;
#317 = DIRECTION ( 'NONE',  ( -0.000000000000000000, -0.000000000000000000, 1.000000000000000000 ) ) ;
#318 = FACE_OUTER_BOUND ( 'NONE', #4303, .T. ) ;
#319 = DIRECTION ( 'NONE',  ( 1.000000000000000000, -0.000000000000000000, -0.000000000000000000 ) ) ;
#320 = ORIENTED_EDGE ( 'NONE', *, *, #6943, .F. ) ;
#321 = ORIENTED_EDGE ( 'NONE', *, *, #9216, .F. ) ;
#322 = LINE ( 'NONE', #3251, #1637 ) ;
#323 = AXIS2_PLACEMENT_3D ( 'NONE', #1612, #9005, #2442 ) ;
#324 = ORIENTED_EDGE ( 'NONE', *, *, #657, .T. ) ;
#325 = EDGE_CURVE ( 'NONE', #3453, #8519, #5765, .T. ) ;
#326 = CARTESIAN_POINT ( 'NONE',  ( 4.000000000000000000, 9.605605015555367541E-13, 18.44000000000276884 ) ) ;
#327 = DIRECTION ( 'NONE',  ( -0.000000000000000000, -0.000000000000000000, -1.000000000000000000 ) ) ;
#328 = EDGE_LOOP ( 'NONE', ( #7572, #3600, #1192, #3524 ) ) ;
#329 =( REPRESENTATION_RELATIONSHIP ('NONE','NONE', #1933, #6964 ) REPRESENTATION_RELATIONSHIP_WITH_TRANSFORMATION ( #8354 )SHAPE_REPRESENTATION_RELATIONSHIP( ) );
#330 = LINE ( 'NONE', #4123, #7938 ) ;
#331 = EDGE_CURVE ( 'NONE', #5110, #5683, #1782, .T. ) ;
#332 = DIRECTION ( 'NONE',  ( 0.000000000000000000, 0.000000000000000000, 1.000000000000000000 ) ) ;
#333 = CARTESIAN_POINT ( 'NONE',  ( 0.000000000000000000, -17.50000000000000000, 49.50000000000000000 ) ) ;
#334 = VERTEX_POINT ( 'NONE', #1065 ) ;
#335 = ORIENTED_EDGE ( 'NONE', *, *, #1536, .T. ) ;
#336 = CIRCLE ( 'NONE', #6014, 0.7499999999989250821 ) ;
#337 = CARTESIAN_POINT ( 'NONE',  ( -27.00000000000000000, -43.00000000000000000, 25.00000000000000000 ) ) ;
#338 = AXIS2_PLACEMENT_3D ( 'NONE', #1148, #4717, #3174 ) ;
#339 = DIRECTION ( 'NONE',  ( -1.000000000000000000, 0.000000000000000000, 0.000000000000000000 ) ) ;
#340 = FILL_AREA_STYLE ('',( #6927 ) ) ;
#341 = CARTESIAN_POINT ( 'NONE',  ( 6.000000000000000888, 22.50000000000000355, 2.000000000000013767 ) ) ;
#342 = PLANE ( 'NONE',  #3730 ) ;
#343 = EDGE_CURVE ( 'NONE', #9037, #2987, #5640, .T. ) ;
#344 = ORIENTED_EDGE ( 'NONE', *, *, #1475, .F. ) ;
#345 = CARTESIAN_POINT ( 'NONE',  ( 40.77961158827727672, -30.00000000000000000, -84.30964406271149869 ) ) ;
#346 = ORIENTED_EDGE ( 'NONE', *, *, #7933, .F. ) ;
#347 = DIRECTION ( 'NONE',  ( 0.000000000000000000, 0.000000000000000000, 1.000000000000000000 ) ) ;
#348 = DIRECTION ( 'NONE',  ( 0.000000000000000000, 0.000000000000000000, -1.000000000000000000 ) ) ;
#349 = EDGE_CURVE ( 'NONE', #1211, #8754, #4001, .T. ) ;
#350 = AXIS2_PLACEMENT_3D ( 'NONE', #1501, #3715, #8755 ) ;
#351 = CARTESIAN_POINT ( 'NONE',  ( -26.99999999999998934, 35.00000000000000000, 5.000000000000004441 ) ) ;
#352 = DIRECTION ( 'NONE',  ( 0.000000000000000000, -1.000000000000000000, 0.000000000000000000 ) ) ;
#353 = ORIENTED_EDGE ( 'NONE', *, *, #5129, .F. ) ;
#354 = ORIENTED_EDGE ( 'NONE', *, *, #1055, .F. ) ;
#355 = EDGE_LOOP ( 'NONE', ( #5445, #2395, #8124, #5569 ) ) ;
#356 = DIRECTION ( 'NONE',  ( -1.000000000000000000, 0.000000000000000000, -0.000000000000000000 ) ) ;
#357 = AXIS2_PLACEMENT_3D ( 'NONE', #2834, #3402, #5045 ) ;
#358 = DIRECTION ( 'NONE',  ( -1.000000000000000000, 0.000000000000000000, 0.000000000000000000 ) ) ;
#359 = LINE ( 'NONE', #3288, #3084 ) ;
#360 = CARTESIAN_POINT ( 'NONE',  ( -6.000000000000000888, 0.000000000000000000, 4.000000000000000000 ) ) ;
#361 = CIRCLE ( 'NONE', #8500, 0.7500000000013684609 ) ;
#362 = DIRECTION ( 'NONE',  ( -0.7071067811865442421, 0.7071067811865509034, 0.000000000000000000 ) ) ;
#363 = ORIENTED_EDGE ( 'NONE', *, *, #6358, .T. ) ;
#364 = ADVANCED_FACE ( 'NONE', ( #3272, #6212 ), #5492, .T. ) ;
#365 = ORIENTED_EDGE ( 'NONE', *, *, #3412, .F. ) ;
#366 = DIRECTION ( 'NONE',  ( -1.000000000000000000, 0.000000000000000000, 0.000000000000000000 ) ) ;
#367 = VERTEX_POINT ( 'NONE', #8420 ) ;
#368 = EDGE_CURVE ( 'NONE', #6290, #8884, #8400, .T. ) ;
#369 = CARTESIAN_POINT ( 'NONE',  ( 26.21170834203230982, -53.97171801779368394, -0.5000000000000038858 ) ) ;
#370 = CARTESIAN_POINT ( 'NONE',  ( 0.000000000000000000, 18.47759065022658120, 7.653668647302884764 ) ) ;
#371 = ORIENTED_EDGE ( 'NONE', *, *, #6027, .F. ) ;
#372 = CARTESIAN_POINT ( 'NONE',  ( 2.499999999999998668, 3.061616997868381662E-16, 21.00000000000000000 ) ) ;
#373 = VECTOR ( 'NONE', #8630, 1000.000000000000000 ) ;
#374 = DIRECTION ( 'NONE',  ( 1.000000000000000000, -0.000000000000000000, -0.000000000000000000 ) ) ;
#375 = CARTESIAN_POINT ( 'NONE',  ( 6.000000000000157208, -22.50000000000000355, 5.000000000000000000 ) ) ;
#376 = ORIENTED_EDGE ( 'NONE', *, *, #2647, .T. ) ;
#377 = AXIS2_PLACEMENT_3D ( 'NONE', #180, #1518, #6041 ) ;
#378 = ORIENTED_EDGE ( 'NONE', *, *, #8438, .T. ) ;
#379 = CONTEXT_DEPENDENT_SHAPE_REPRESENTATION ( #5607, #864 ) ;
#380 = CARTESIAN_POINT ( 'NONE',  ( 0.000000000000000000, -22.50000000000000355, 0.000000000000000000 ) ) ;
#381 = AXIS2_PLACEMENT_3D ( 'NONE', #4618, #6925, #3129 ) ;
#382 = FACE_OUTER_BOUND ( 'NONE', #2751, .T. ) ;
#383 = DIRECTION ( 'NONE',  ( 1.000000000000000000, 0.000000000000000000, 0.000000000000000000 ) ) ;
#384 = DIRECTION ( 'NONE',  ( -1.000000000000000000, -0.000000000000000000, -0.000000000000000000 ) ) ;
#385 = LINE ( 'NONE', #9079, #8335 ) ;
#386 = VERTEX_POINT ( 'NONE', #3317 ) ;
#387 = DIRECTION ( 'NONE',  ( -1.000000000000000000, 0.000000000000000000, 0.000000000000000000 ) ) ;
#388 =( BOUNDED_CURVE ( )  B_SPLINE_CURVE ( 3, ( #3943, #6883, #7691, #297 ),
 .UNSPECIFIED., .F., .T. ) 
 B_SPLINE_CURVE_WITH_KNOTS ( ( 4, 4 ),
 ( 0.000000000000000000, 0.7853981633974483900 ),
 .UNSPECIFIED. ) 
 CURVE ( )  GEOMETRIC_REPRESENTATION_ITEM ( )  RATIONAL_B_SPLINE_CURVE ( ( 1.000000000000000000, 0.9492530216741911220, 0.9492530216741911220, 1.000000000000000000 ) ) 
 REPRESENTATION_ITEM ( '' )  );
#389 = ORIENTED_EDGE ( 'NONE', *, *, #8426, .T. ) ;
#390 = CARTESIAN_POINT ( 'NONE',  ( 0.000000000000000000, 20.00000000000120437, 1.559999999999680531 ) ) ;
#391 = FACE_OUTER_BOUND ( 'NONE', #7169, .T. ) ;
#392 = CARTESIAN_POINT ( 'NONE',  ( 0.000000000000000000, 0.000000000000000000, 0.000000000000000000 ) ) ;
#393 = DIRECTION ( 'NONE',  ( 0.000000000000000000, 0.000000000000000000, 1.000000000000000000 ) ) ;
#394 = ORIENTED_EDGE ( 'NONE', *, *, #228, .T. ) ;
#395 = AXIS2_PLACEMENT_3D ( 'NONE', #3027, #5818, #6637 ) ;
#396 = ADVANCED_FACE ( 'NONE', ( #2058, #4983 ), #8012, .T. ) ;
#397 = ORIENTED_EDGE ( 'NONE', *, *, #2413, .T. ) ;
#398 = CARTESIAN_POINT ( 'NONE',  ( 0.000000000000000000, 0.000000000000000000, 0.000000000000000000 ) ) ;
#399 = ORIENTED_EDGE ( 'NONE', *, *, #3163, .F. ) ;
#400 = CARTESIAN_POINT ( 'NONE',  ( -27.00000000000000000, 43.00000000000000000, -25.00000000000000000 ) ) ;
#401 = LINE ( 'NONE', #6284, #5327 ) ;
#402 = DIRECTION ( 'NONE',  ( -1.000000000000000000, 0.000000000000000000, 0.000000000000000000 ) ) ;
#403 = AXIS2_PLACEMENT_3D ( 'NONE', #1611, #2187, #4396 ) ;
#404 = CIRCLE ( 'NONE', #2411, 11.96410161513786008 ) ;
#405 = CARTESIAN_POINT ( 'NONE',  ( -17.50000000000000355, 2.143131898507868643E-15, 49.50000000000000000 ) ) ;
#406 = CARTESIAN_POINT ( 'NONE',  ( -6.000000000000000888, 22.50000000000000355, 5.000000000000000000 ) ) ;
#407 = ADVANCED_FACE ( 'NONE', ( #6580 ), #3012, .F. ) ;
#408 = EDGE_LOOP ( 'NONE', ( #6150, #3205, #7660, #2925 ) ) ;
#409 = DIRECTION ( 'NONE',  ( 0.000000000000000000, 0.000000000000000000, 1.000000000000000000 ) ) ;
#410 = VERTEX_POINT ( 'NONE', #8203 ) ;
#411 = VECTOR ( 'NONE', #1740, 1000.000000000000000 ) ;
#412 = ORIENTED_EDGE ( 'NONE', *, *, #8365, .F. ) ;
#413 = DIRECTION ( 'NONE',  ( -1.000000000000000000, 0.000000000000000000, -0.000000000000000000 ) ) ;
#414 = AXIS2_PLACEMENT_3D ( 'NONE', #5872, #8891, #919 ) ;
#415 = FACE_OUTER_BOUND ( 'NONE', #1978, .T. ) ;
#416 = VECTOR ( 'NONE', #4660, 1000.000000000000114 ) ;
#417 = AXIS2_PLACEMENT_3D ( 'NONE', #8112, #7380, #7479 ) ;
#418 = VECTOR ( 'NONE', #675, 1000.000000000000000 ) ;
#419 = EDGE_CURVE ( 'NONE', #5419, #3913, #3949, .T. ) ;
#420 = LINE ( 'NONE', #3394, #982 ) ;
#421 = LINE ( 'NONE', #3354, #4265 ) ;
#422 = VECTOR ( 'NONE', #8302, 1000.000000000000000 ) ;
#423 = ADVANCED_FACE ( 'NONE', ( #6672 ), #1620, .F. ) ;
#424 = VERTEX_POINT ( 'NONE', #2296 ) ;
#425 = ORIENTED_EDGE ( 'NONE', *, *, #6234, .F. ) ;
#426 = EDGE_CURVE ( 'NONE', #7367, #6082, #2257, .T. ) ;
#427 = EDGE_CURVE ( 'NONE', #424, #3685, #1571, .T. ) ;
#428 = VECTOR ( 'NONE', #1377, 1000.000000000000000 ) ;
#429 = SHAPE_DEFINITION_REPRESENTATION ( #1557, #6964 ) ;
#430 = DIRECTION ( 'NONE',  ( 0.000000000000000000, -0.000000000000000000, -1.000000000000000000 ) ) ;
#431 = CIRCLE ( 'NONE', #2590, 6.000000000000000888 ) ;
#432 = DIRECTION ( 'NONE',  ( -0.000000000000000000, -0.000000000000000000, -1.000000000000000000 ) ) ;
#433 = CARTESIAN_POINT ( 'NONE',  ( 12.37436867076458036, -12.37436867076458036, 19.62563132923542142 ) ) ;
#434 = DIRECTION ( 'NONE',  ( -0.000000000000000000, -0.000000000000000000, -1.000000000000000000 ) ) ;
#435 = EDGE_CURVE ( 'NONE', #2310, #1809, #3699, .T. ) ;
#436 = CARTESIAN_POINT ( 'NONE',  ( -12.37436867076458036, 12.37436867076458036, 19.62563132923542142 ) ) ;
#437 = EDGE_CURVE ( 'NONE', #7541, #6226, #115, .T. ) ;
#438 = VERTEX_POINT ( 'NONE', #1523 ) ;
#439 = AXIS2_PLACEMENT_3D ( 'NONE', #3196, #888, #5313 ) ;
#440 = ORIENTED_EDGE ( 'NONE', *, *, #6665, .T. ) ;
#441 = EDGE_CURVE ( 'NONE', #2574, #8783, #903, .T. ) ;
#442 = AXIS2_PLACEMENT_3D ( 'NONE', #1442, #3660, #4332 ) ;
#443 = CARTESIAN_POINT ( 'NONE',  ( 31.00000000000002132, 0.000000000000000000, 32.00000000000000000 ) ) ;
#444 = CARTESIAN_POINT ( 'NONE',  ( -27.00000000000000000, -43.00000000000000000, 11.99999999999999645 ) ) ;
#445 = CARTESIAN_POINT ( 'NONE',  ( -27.00000000000000000, -43.00000000000000000, 11.99999999999999645 ) ) ;
#446 = CARTESIAN_POINT ( 'NONE',  ( -38.00000000000000711, -43.00000000000000000, -7.366666666666667140 ) ) ;
#447 = AXIS2_PLACEMENT_3D ( 'NONE', #6686, #8219, #4473 ) ;
#448 = FACE_OUTER_BOUND ( 'NONE', #1573, .T. ) ;
#449 = ORIENTED_EDGE ( 'NONE', *, *, #3589, .T. ) ;
#450 = VERTEX_POINT ( 'NONE', #87 ) ;
#451 = DIRECTION ( 'NONE',  ( 1.000000000000000000, 0.000000000000000000, 0.000000000000000000 ) ) ;
#452 = ORIENTED_EDGE ( 'NONE', *, *, #7402, .F. ) ;
#453 = DIRECTION ( 'NONE',  ( 1.000000000000000000, 0.000000000000000000, 0.000000000000000000 ) ) ;
#454 = DIRECTION ( 'NONE',  ( 0.000000000000000000, 1.000000000000000000, 0.000000000000000000 ) ) ;
#455 = DIRECTION ( 'NONE',  ( 0.000000000000000000, 0.7071067811865479058, -0.7071067811865472397 ) ) ;
#456 = CARTESIAN_POINT ( 'NONE',  ( -28.50000000000000000, -7.855833012397050680E-14, 5.000000000000000000 ) ) ;
#457 = DIRECTION ( 'NONE',  ( 0.000000000000000000, 0.000000000000000000, 1.000000000000000000 ) ) ;
#458 = VERTEX_POINT ( 'NONE', #5126 ) ;
#459 = ORIENTED_EDGE ( 'NONE', *, *, #6511, .F. ) ;
#460 = DIRECTION ( 'NONE',  ( 1.000000000000000000, 0.000000000000000000, 0.000000000000000000 ) ) ;
#461 = ORIENTED_EDGE ( 'NONE', *, *, #4475, .T. ) ;
#462 = EDGE_CURVE ( 'NONE', #5577, #4499, #9447, .T. ) ;
#463 = LINE ( 'NONE', #6333, #3982 ) ;
#464 = DIRECTION ( 'NONE',  ( 0.000000000000000000, 0.000000000000000000, -1.000000000000000000 ) ) ;
#465 = ORIENTED_EDGE ( 'NONE', *, *, #9033, .T. ) ;
#466 = DIRECTION ( 'NONE',  ( -0.5773502691896283956, 0.5773502691896229555, 0.5773502691896260641 ) ) ;
#467 = DIRECTION ( 'NONE',  ( 0.000000000000000000, 0.000000000000000000, 1.000000000000000000 ) ) ;
#468 = CARTESIAN_POINT ( 'NONE',  ( -5.999999999999842792, -22.50000000000000355, 0.000000000000000000 ) ) ;
#469 = CONICAL_SURFACE ( 'NONE', #1852, 18.49999999999998934, 0.7853981633974517207 ) ;
#470 = CARTESIAN_POINT ( 'NONE',  ( 28.21791960234944341, 3.296518076058924773, 1.407948315796077488 ) ) ;
#471 = ORIENTED_EDGE ( 'NONE', *, *, #2053, .F. ) ;
#472 = VERTEX_POINT ( 'NONE', #2965 ) ;
#473 = CIRCLE ( 'NONE', #8880, 11.00000000000000000 ) ;
#474 = EDGE_CURVE ( 'NONE', #1673, #5235, #848, .T. ) ;
#475 = ADVANCED_FACE ( 'NONE', ( #756 ), #4106, .T. ) ;
#476 = CARTESIAN_POINT ( 'NONE',  ( -37.00000000000000711, -15.90990257669733943, -85.90990257669729147 ) ) ;
#477 = LINE ( 'NONE', #4853, #2042 ) ;
#478 = DIRECTION ( 'NONE',  ( 0.7071067811865474617, 0.000000000000000000, -0.7071067811865474617 ) ) ;
#479 = EDGE_LOOP ( 'NONE', ( #8954, #2273 ) ) ;
#480 = ORIENTED_EDGE ( 'NONE', *, *, #2220, .T. ) ;
#481 = ORIENTED_EDGE ( 'NONE', *, *, #7216, .T. ) ;
#482 = ORIENTED_EDGE ( 'NONE', *, *, #2518, .F. ) ;
#483 = EDGE_CURVE ( 'NONE', #1534, #3407, #8098, .T. ) ;
#484 = DIRECTION ( 'NONE',  ( -1.000000000000000000, 0.000000000000000000, 0.000000000000000000 ) ) ;
#485 = CIRCLE ( 'NONE', #2499, 17.50000000000000000 ) ;
#486 = DIRECTION ( 'NONE',  ( -1.000000000000000000, 0.000000000000000000, 0.000000000000000000 ) ) ;
#487 = DIRECTION ( 'NONE',  ( 0.000000000000000000, 0.000000000000000000, 1.000000000000000000 ) ) ;
#488 = EDGE_CURVE ( 'NONE', #9116, #6136, #6414, .T. ) ;
#489 = CARTESIAN_POINT ( 'NONE',  ( -19.74999999999999645, 43.00000000000000000, 25.00000000000000000 ) ) ;
#490 = VERTEX_POINT ( 'NONE', #2874 ) ;
#491 = ORIENTED_EDGE ( 'NONE', *, *, #4676, .F. ) ;
#492 = CARTESIAN_POINT ( 'NONE',  ( 7.219041098785710986, 44.46340980410260357, 44.81174454080558434 ) ) ;
#493 = ORIENTED_EDGE ( 'NONE', *, *, #6896, .F. ) ;
#494 = FACE_BOUND ( 'NONE', #302, .T. ) ;
#495 = VECTOR ( 'NONE', #924, 1000.000000000000000 ) ;
#496 = DIRECTION ( 'NONE',  ( 0.000000000000000000, 0.000000000000000000, 1.000000000000000000 ) ) ;
#497 = CARTESIAN_POINT ( 'NONE',  ( -40.77961158827728383, -30.00000000000000000, -84.30964406271149869 ) ) ;
#498 = CARTESIAN_POINT ( 'NONE',  ( 5.000000000000000000, -18.47759065022712832, 6.903668647304566974 ) ) ;
#499 = APPLICATION_CONTEXT ( 'automotive_design' ) ;
#500 = CIRCLE ( 'NONE', #2957, 8.000000000000021316 ) ;
#501 = CARTESIAN_POINT ( 'NONE',  ( 22.50000000000000355, 0.000000000000000000, 10.00000000000000000 ) ) ;
#502 = ORIENTED_EDGE ( 'NONE', *, *, #6422, .F. ) ;
#503 = EDGE_LOOP ( 'NONE', ( #6940, #1509 ) ) ;
#504 = CARTESIAN_POINT ( 'NONE',  ( -4.333301281932778082, 26.64999999999997371, 0.000000000000000000 ) ) ;
#505 = ORIENTED_EDGE ( 'NONE', *, *, #4882, .F. ) ;
#506 = CARTESIAN_POINT ( 'NONE',  ( 0.000000000000000000, -22.50000000000000355, 10.00000000000000000 ) ) ;
#507 = CARTESIAN_POINT ( 'NONE',  ( 19.74999999999999645, 43.00000000000000000, 11.99999999999999645 ) ) ;
#508 = DIRECTION ( 'NONE',  ( -1.000000000000000000, -0.000000000000000000, -0.000000000000000000 ) ) ;
#509 = DIRECTION ( 'NONE',  ( 0.000000000000000000, 0.000000000000000000, 1.000000000000000000 ) ) ;
#510 = CIRCLE ( 'NONE', #7729, 2.999999999999999112 ) ;
#511 = ADVANCED_FACE ( 'NONE', ( #5806 ), #9311, .T. ) ;
#512 = CARTESIAN_POINT ( 'NONE',  ( 60.00000000000000000, 15.90990257669733943, -54.09009742330271564 ) ) ;
#513 = CARTESIAN_POINT ( 'NONE',  ( 28.66635145370233673, 1.351859493328352091, 1.696225934522933132 ) ) ;
#514 = ORIENTED_EDGE ( 'NONE', *, *, #8952, .T. ) ;
#515 = ORIENTED_EDGE ( 'NONE', *, *, #5543, .T. ) ;
#516 = EDGE_CURVE ( 'NONE', #1904, #3854, #5179, .T. ) ;
#517 = CONTEXT_DEPENDENT_SHAPE_REPRESENTATION ( #6222, #9284 ) ;
#518 = VECTOR ( 'NONE', #1188, 1000.000000000000000 ) ;
#519 = FACE_OUTER_BOUND ( 'NONE', #8224, .T. ) ;
#520 = AXIS2_PLACEMENT_3D ( 'NONE', #2674, #6231, #6948 ) ;
#521 = CARTESIAN_POINT ( 'NONE',  ( 37.00000000000000000, 15.90990257669733943, -82.90990257669729147 ) ) ;
#522 = CARTESIAN_POINT ( 'NONE',  ( -53.29490495164537833, 27.56180520566615044, -81.40266088840108694 ) ) ;
#523 = VERTEX_POINT ( 'NONE', #5519 ) ;
#524 = ORIENTED_EDGE ( 'NONE', *, *, #7444, .F. ) ;
#525 = AXIS2_PLACEMENT_3D ( 'NONE', #6666, #83, #3007 ) ;
#526 = EDGE_LOOP ( 'NONE', ( #3501, #2271 ) ) ;
#527 = CARTESIAN_POINT ( 'NONE',  ( -34.25000000000000000, 43.00000000000000000, 25.00000000000000000 ) ) ;
#528 = VECTOR ( 'NONE', #5678, 1000.000000000000000 ) ;
#529 = DIRECTION ( 'NONE',  ( 0.000000000000000000, 0.000000000000000000, -1.000000000000000000 ) ) ;
#531 = FACE_OUTER_BOUND ( 'NONE', #7505, .T. ) ;
#530 = PRODUCT_RELATED_PRODUCT_CATEGORY ( 'part', '', ( #5855 ) ) ;
#532 = ADVANCED_FACE ( 'NONE', ( #1086 ), #4027, .T. ) ;
#533 = FACE_OUTER_BOUND ( 'NONE', #4151, .T. ) ;
#534 = ADVANCED_FACE ( 'NONE', ( #8448, #1718, #6196, #5421, #992, #3880 ), #1862, .T. ) ;
#535 = EDGE_CURVE ( 'NONE', #3097, #7881, #1674, .T. ) ;
#536 = FACE_BOUND ( 'NONE', #7103, .T. ) ;
#537 = ORIENTED_EDGE ( 'NONE', *, *, #8121, .T. ) ;
#538 = CARTESIAN_POINT ( 'NONE',  ( 0.7500000000000000000, -0.7500000000000000000, 1.500000000000000000 ) ) ;
#539 = DIRECTION ( 'NONE',  ( -1.000000000000000000, 0.000000000000000000, 0.000000000000000000 ) ) ;
#540 = EDGE_CURVE ( 'NONE', #4866, #6634, #4500, .T. ) ;
#541 = ORIENTED_EDGE ( 'NONE', *, *, #549, .F. ) ;
#542 = FACE_BOUND ( 'NONE', #564, .T. ) ;
#543 = CARTESIAN_POINT ( 'NONE',  ( -17.50000000000000355, 2.143131898507868643E-15, 14.49999999999999822 ) ) ;
#544 = DIRECTION ( 'NONE',  ( -0.000000000000000000, -0.000000000000000000, -1.000000000000000000 ) ) ;
#545 = DIRECTION ( 'NONE',  ( -0.000000000000000000, -0.000000000000000000, -1.000000000000000000 ) ) ;
#546 = AXIS2_PLACEMENT_3D ( 'NONE', #1226, #8727, #4975 ) ;
#547 = DIRECTION ( 'NONE',  ( -0.000000000000000000, -0.000000000000000000, -1.000000000000000000 ) ) ;
#548 = ORIENTED_EDGE ( 'NONE', *, *, #1293, .T. ) ;
#549 = EDGE_CURVE ( 'NONE', #1368, #849, #2819, .T. ) ;
#550 = VERTEX_POINT ( 'NONE', #234 ) ;
#551 = DIRECTION ( 'NONE',  ( 1.000000000000000000, -0.000000000000000000, -0.000000000000000000 ) ) ;
#552 = ORIENTED_EDGE ( 'NONE', *, *, #7615, .F. ) ;
#553 = EDGE_CURVE ( 'NONE', #4380, #6251, #3112, .T. ) ;
#554 = DIRECTION ( 'NONE',  ( 1.000000000000000000, 0.000000000000000000, 0.000000000000000000 ) ) ;
#555 = LINE ( 'NONE', #9438, #7175 ) ;
#556 = ADVANCED_FACE ( 'NONE', ( #2453, #6048, #4749, #8968, #2397, #5469 ), #3297, .T. ) ;
#557 = DIRECTION ( 'NONE',  ( -1.000000000000000000, -0.000000000000000000, -0.000000000000000000 ) ) ;
#558 = CONICAL_SURFACE ( 'NONE', #5167, 30.00000000000000000, 0.7853981633974428389 ) ;
#559 = CARTESIAN_POINT ( 'NONE',  ( 37.00000000000000000, 15.90990257669733943, -88.90990257669730568 ) ) ;
#560 = CARTESIAN_POINT ( 'NONE',  ( 4.000000000000000000, 9.603694566548697359E-13, 20.00000000000290612 ) ) ;
#561 = CARTESIAN_POINT ( 'NONE',  ( -7.180166011355011868, -26.02777777777776791, 0.000000000000000000 ) ) ;
#562 = VECTOR ( 'NONE', #7217, 1000.000000000000000 ) ;
#563 = ORIENTED_EDGE ( 'NONE', *, *, #154, .F. ) ;
#564 = EDGE_LOOP ( 'NONE', ( #4650, #3355 ) ) ;
#565 = CARTESIAN_POINT ( 'NONE',  ( -25.50000000000000000, -7.855833012397050680E-14, 15.00000000000000000 ) ) ;
#566 = ITEM_DEFINED_TRANSFORMATION ( 'NONE', 'NONE', #7443,  #1614 ) ;
#567 = VECTOR ( 'NONE', #150, 999.9999999999998863 ) ;
#568 = AXIS2_PLACEMENT_3D ( 'NONE', #1834, #4046, #387 ) ;
#569 = DIRECTION ( 'NONE',  ( -0.000000000000000000, 1.000000000000000000, -0.000000000000000000 ) ) ;
#570 = CONICAL_SURFACE ( 'NONE', #6720, 59.00000000000000000, 0.7853981633974415066 ) ;
#571 = CARTESIAN_POINT ( 'NONE',  ( 0.000000000000000000, 22.50000000000000355, 5.000000000000000000 ) ) ;
#572 = CIRCLE ( 'NONE', #5484, 7.250000000000002665 ) ;
#573 = CARTESIAN_POINT ( 'NONE',  ( -26.99999999999998934, 29.99999999999997158, 64.00000000000000000 ) ) ;
#574 = LINE ( 'NONE', #7151, #8849 ) ;
#575 = AXIS2_PLACEMENT_3D ( 'NONE', #1520, #5762, #8108 ) ;
#576 = ORIENTED_EDGE ( 'NONE', *, *, #1236, .F. ) ;
#577 = ORIENTED_EDGE ( 'NONE', *, *, #844, .F. ) ;
#578 = EDGE_LOOP ( 'NONE', ( #1745, #6700, #5279, #2448 ) ) ;
#579 = AXIS2_PLACEMENT_3D ( 'NONE', #3294, #9015, #8255 ) ;
#580 = VERTEX_POINT ( 'NONE', #8394 ) ;
#581 = DIRECTION ( 'NONE',  ( -0.7071067811865505703, -0.7071067811865444641, 0.000000000000000000 ) ) ;
#582 = AXIS2_PLACEMENT_3D ( 'NONE', #2681, #3390, #5663 ) ;
#583 = CARTESIAN_POINT ( 'NONE',  ( 0.000000000000000000, 0.000000000000000000, 10.00000000000000000 ) ) ;
#584 = DIRECTION ( 'NONE',  ( -0.000000000000000000, -0.000000000000000000, 1.000000000000000000 ) ) ;
#585 = FACE_OUTER_BOUND ( 'NONE', #9353, .T. ) ;
#586 = FACE_BOUND ( 'NONE', #5148, .T. ) ;
#587 = VECTOR ( 'NONE', #7326, 1000.000000000000000 ) ;
#588 = ORIENTED_EDGE ( 'NONE', *, *, #4774, .F. ) ;
#589 = AXIS2_PLACEMENT_3D ( 'NONE', #8025, #3797, #1585 ) ;
#590 = DIRECTION ( 'NONE',  ( 0.7071067811865490160, -0.7071067811865461294, 0.000000000000000000 ) ) ;
#591 = ORIENTED_EDGE ( 'NONE', *, *, #5521, .F. ) ;
#592 = FACE_OUTER_BOUND ( 'NONE', #5726, .T. ) ;
#593 = CARTESIAN_POINT ( 'NONE',  ( 32.00000000000000711, 29.99999999999997868, 64.00000000000000000 ) ) ;
#594 = EDGE_CURVE ( 'NONE', #5792, #8082, #284, .T. ) ;
#595 = CARTESIAN_POINT ( 'NONE',  ( -15.00000000000000000, 0.000000000000000000, 20.00000000000000000 ) ) ;
#596 = ADVANCED_FACE ( 'NONE', ( #3209, #947, #3160, #6099, #7678, #2538 ), #2588, .T. ) ;
#597 = LINE ( 'NONE', #688, #3837 ) ;
#598 = EDGE_CURVE ( 'NONE', #3092, #1471, #8300, .T. ) ;
#599 = ADVANCED_FACE ( 'NONE', ( #4699 ), #7576, .T. ) ;
#600 = CARTESIAN_POINT ( 'NONE',  ( 32.00000000000000711, -29.99999999999996447, 58.99999999999997158 ) ) ;
#601 = ORIENTED_EDGE ( 'NONE', *, *, #5718, .F. ) ;
#602 = VERTEX_POINT ( 'NONE', #326 ) ;
#603 = CARTESIAN_POINT ( 'NONE',  ( -38.00000000000000711, 43.00000000000000000, -7.366666666666667140 ) ) ;
#604 = EDGE_LOOP ( 'NONE', ( #1437, #3375 ) ) ;
#605 = DIRECTION ( 'NONE',  ( 0.000000000000000000, 0.000000000000000000, 1.000000000000000000 ) ) ;
#606 = DIRECTION ( 'NONE',  ( 1.000000000000000000, 0.000000000000000000, 0.000000000000000000 ) ) ;
#607 = CARTESIAN_POINT ( 'NONE',  ( 0.000000000000000000, 14.14213562373247868, 14.14213562373282329 ) ) ;
#608 = EDGE_CURVE ( 'NONE', #8189, #5235, #3253, .T. ) ;
#609 = CARTESIAN_POINT ( 'NONE',  ( 5.000000000000000000, 18.47759065022580316, -8.403668647301632433 ) ) ;
#610 = AXIS2_PLACEMENT_3D ( 'NONE', #5055, #7982, #487 ) ;
#611 = CARTESIAN_POINT ( 'NONE',  ( -15.99999999999999645, 43.00000000000000000, 11.99999999999999645 ) ) ;
#612 = CYLINDRICAL_SURFACE ( 'NONE', #5951, 6.000000000000000000 ) ;
#613 = EDGE_CURVE ( 'NONE', #2492, #9459, #3813, .T. ) ;
#614 = ORIENTED_EDGE ( 'NONE', *, *, #5661, .F. ) ;
#615 = ORIENTED_EDGE ( 'NONE', *, *, #540, .F. ) ;
#616 = CYLINDRICAL_SURFACE ( 'NONE', #3643, 0.7499999999989250821 ) ;
#617 = CONTEXT_DEPENDENT_SHAPE_REPRESENTATION ( #2659, #2013 ) ;
#618 = EDGE_LOOP ( 'NONE', ( #4877, #690, #1083, #7069 ) ) ;
#619 = ADVANCED_FACE ( 'NONE', ( #5567 ), #6285, .T. ) ;
#620 = DIRECTION ( 'NONE',  ( 0.000000000000000000, 0.000000000000000000, 1.000000000000000000 ) ) ;
#621 = CIRCLE ( 'NONE', #9367, 2.999999999999999556 ) ;
#622 = CARTESIAN_POINT ( 'NONE',  ( 12.37436867076458036, -12.37436867076458036, 19.62563132923542142 ) ) ;
#623 = CARTESIAN_POINT ( 'NONE',  ( 5.000000000000000888, 0.000000000000000000, 1.000000000000000000 ) ) ;
#624 = ORIENTED_EDGE ( 'NONE', *, *, #5824, .T. ) ;
#625 = ORIENTED_EDGE ( 'NONE', *, *, #1373, .T. ) ;
#626 = EDGE_LOOP ( 'NONE', ( #6551, #3598, #3305, #7283, #8776 ) ) ;
#627 = AXIS2_PLACEMENT_3D ( 'NONE', #6856, #4109, #1035 ) ;
#628 = ORIENTED_EDGE ( 'NONE', *, *, #7466, .T. ) ;
#629 = CARTESIAN_POINT ( 'NONE',  ( 60.00000000000000000, -15.90990257669733943, -85.90990257669729147 ) ) ;
#630 = CARTESIAN_POINT ( 'NONE',  ( 0.000000000000000000, 22.50000000000000355, 0.000000000000000000 ) ) ;
#631 = CARTESIAN_POINT ( 'NONE',  ( 30.00000000000000000, 3.673940397442059178E-15, 8.000000000000005329 ) ) ;
#632 = CARTESIAN_POINT ( 'NONE',  ( 3.000000000000000000, 22.50000000000000355, 5.000000000000000000 ) ) ;
#633 = EDGE_CURVE ( 'NONE', #6290, #6045, #8491, .T. ) ;
#634 = DIRECTION ( 'NONE',  ( 1.000000000000000000, 0.000000000000000000, 0.000000000000000000 ) ) ;
#635 = ORIENTED_EDGE ( 'NONE', *, *, #1121, .F. ) ;
#636 = CARTESIAN_POINT ( 'NONE',  ( -53.29490495164537833, -48.67545040036925741, -60.28901569369804747 ) ) ;
#637 = ORIENTED_EDGE ( 'NONE', *, *, #2315, .F. ) ;
#638 = VECTOR ( 'NONE', #352, 1000.000000000000000 ) ;
#639 = PLANE ( 'NONE',  #3264 ) ;
#640 = EDGE_CURVE ( 'NONE', #410, #2498, #1672, .T. ) ;
#641 = CARTESIAN_POINT ( 'NONE',  ( 0.000000000000000000, 0.000000000000000000, 3.000000000000052847 ) ) ;
#642 =( BOUNDED_CURVE ( )  B_SPLINE_CURVE ( 3, ( #1543, #1590, #161, #2983 ),
 .UNSPECIFIED., .F., .T. ) 
 B_SPLINE_CURVE_WITH_KNOTS ( ( 4, 4 ),
 ( 2.356194490192344837, 3.141592653589793116 ),
 .UNSPECIFIED. ) 
 CURVE ( )  GEOMETRIC_REPRESENTATION_ITEM ( )  RATIONAL_B_SPLINE_CURVE ( ( 1.000000000000000000, 0.9492530216741911220, 0.9492530216741911220, 1.000000000000000000 ) ) 
 REPRESENTATION_ITEM ( '' )  );
#643 = CARTESIAN_POINT ( 'NONE',  ( 0.000000000000000000, 22.50000000000000355, 5.000000000000000000 ) ) ;
#644 = CARTESIAN_POINT ( 'NONE',  ( 27.00000000000000355, -34.99999999999999289, 5.000000000000004441 ) ) ;
#645 = VECTOR ( 'NONE', #5294, 1000.000000000000000 ) ;
#646 = DIRECTION ( 'NONE',  ( 0.000000000000000000, 0.000000000000000000, -1.000000000000000000 ) ) ;
#647 = ORIENTED_EDGE ( 'NONE', *, *, #2998, .F. ) ;
#648 = ORIENTED_EDGE ( 'NONE', *, *, #5543, .F. ) ;
#649 = CARTESIAN_POINT ( 'NONE',  ( -51.96152422706632734, -30.00000000000000000, -134.0000000000000284 ) ) ;
#650 = VECTOR ( 'NONE', #212, 1000.000000000000000 ) ;
#651 = VERTEX_POINT ( 'NONE', #8582 ) ;
#652 = LINE ( 'NONE', #6703, #1819 ) ;
#653 = LINE ( 'NONE', #6518, #4120 ) ;
#654 = CARTESIAN_POINT ( 'NONE',  ( 1.749999999999997780, -1.750000000000013101, 0.000000000000000000 ) ) ;
#655 = CARTESIAN_POINT ( 'NONE',  ( -3.000000000000000000, 22.50000000000000355, 10.00000000000000000 ) ) ;
#656 = AXIS2_PLACEMENT_3D ( 'NONE', #6323, #2670, #8522 ) ;
#657 = EDGE_CURVE ( 'NONE', #4079, #8518, #4927, .T. ) ;
#658 = CARTESIAN_POINT ( 'NONE',  ( 4.000000000000000000, -18.47759065022712832, 7.653668647304757044 ) ) ;
#659 = FACE_OUTER_BOUND ( 'NONE', #8233, .T. ) ;
#660 = ADVANCED_FACE ( 'NONE', ( #8624 ), #2088, .F. ) ;
#661 = ORIENTED_EDGE ( 'NONE', *, *, #8541, .F. ) ;
#662 = VERTEX_POINT ( 'NONE', #4972 ) ;
#663 = LINE ( 'NONE', #1331, #1493 ) ;
#664 = VECTOR ( 'NONE', #7045, 1000.000000000000000 ) ;
#665 = CARTESIAN_POINT ( 'NONE',  ( 19.00000000000000000, 1.673048428422632513E-15, -13.66147716702868031 ) ) ;
#666 = CARTESIAN_POINT ( 'NONE',  ( 60.00000000000000000, -30.00000000000000355, -82.50000000000001421 ) ) ;
#667 = DIRECTION ( 'NONE',  ( 0.000000000000000000, 0.000000000000000000, 1.000000000000000000 ) ) ;
#668 = ORIENTED_EDGE ( 'NONE', *, *, #3534, .T. ) ;
#669 = AXIS2_PLACEMENT_3D ( 'NONE', #44, #3585, #3155 ) ;
#670 = EDGE_LOOP ( 'NONE', ( #399, #371, #4638, #1647, #934, #6701, #9260, #4002 ) ) ;
#671 = ORIENTED_EDGE ( 'NONE', *, *, #5315, .T. ) ;
#672 = VERTEX_POINT ( 'NONE', #7860 ) ;
#673 = CONICAL_SURFACE ( 'NONE', #7266, 18.50000000000001776, 0.7853981633974431720 ) ;
#674 = DIRECTION ( 'NONE',  ( 0.7071067811865441310, -0.7071067811865510144, 0.000000000000000000 ) ) ;
#675 = DIRECTION ( 'NONE',  ( 0.000000000000000000, 0.000000000000000000, -1.000000000000000000 ) ) ;
#676 = CARTESIAN_POINT ( 'NONE',  ( 53.29490495164537833, 15.90990257669733943, -54.09009742330271564 ) ) ;
#677 = CARTESIAN_POINT ( 'NONE',  ( 0.000000000000000000, 30.00000000000000000, 0.000000000000000000 ) ) ;
#678 = FACE_BOUND ( 'NONE', #2572, .T. ) ;
#679 = AXIS2_PLACEMENT_3D ( 'NONE', #8913, #3105, #4816 ) ;
#680 = CARTESIAN_POINT ( 'NONE',  ( 5.000000000000000000, 7.653668647302530381, 18.47759065022802716 ) ) ;
#681 = EDGE_LOOP ( 'NONE', ( #2078, #3194, #2258, #7181 ) ) ;
#682 = CARTESIAN_POINT ( 'NONE',  ( 4.000000000000000888, 0.000000000000000000, 0.000000000000000000 ) ) ;
#683 = ORIENTED_EDGE ( 'NONE', *, *, #6737, .T. ) ;
#684 =( REPRESENTATION_RELATIONSHIP ('NONE','NONE', #1933, #8501 ) REPRESENTATION_RELATIONSHIP_WITH_TRANSFORMATION ( #2648 )SHAPE_REPRESENTATION_RELATIONSHIP( ) );
#685 = CARTESIAN_POINT ( 'NONE',  ( 38.00000000000000711, 21.00000000000000000, -16.89999999999999858 ) ) ;
#686 = CARTESIAN_POINT ( 'NONE',  ( 22.50000000000000355, 0.000000000000000000, 10.00000000000000000 ) ) ;
#687 = DIRECTION ( 'NONE',  ( -1.000000000000000000, 0.000000000000000000, 0.000000000000000000 ) ) ;
#688 = CARTESIAN_POINT ( 'NONE',  ( -52.83333333333332860, 1.666666666666670515, -110.8333333333333570 ) ) ;
#689 = CARTESIAN_POINT ( 'NONE',  ( 2.081312099201997334, -28.14194242914269140, 1.216216932313274102 ) ) ;
#690 = ORIENTED_EDGE ( 'NONE', *, *, #4956, .T. ) ;
#691 = VECTOR ( 'NONE', #2336, 1000.000000000000000 ) ;
#692 = ORIENTED_EDGE ( 'NONE', *, *, #1393, .T. ) ;
#693 = CARTESIAN_POINT ( 'NONE',  ( 4.333301281932778082, 26.64999999999997371, 0.000000000000000000 ) ) ;
#694 = VERTEX_POINT ( 'NONE', #1906 ) ;
#695 = CARTESIAN_POINT ( 'NONE',  ( -28.40898306695984843, -1.062480114423898225, 1.428075945201411789 ) ) ;
#696 = DIRECTION ( 'NONE',  ( -0.000000000000000000, -0.000000000000000000, -1.000000000000000000 ) ) ;
#697 = CARTESIAN_POINT ( 'NONE',  ( 4.000000000000000000, 7.653668647300657213, -18.47759065022568237 ) ) ;
#698 = CYLINDRICAL_SURFACE ( 'NONE', #2313, 3.000000000000000000 ) ;
#699 = ORIENTED_EDGE ( 'NONE', *, *, #1430, .T. ) ;
#700 = EDGE_CURVE ( 'NONE', #4346, #4647, #8117, .T. ) ;
#701 = LINE ( 'NONE', #751, #6370 ) ;
#702 = CARTESIAN_POINT ( 'NONE',  ( 2.749999999999996447, -0.7500000000000000000, 1.500000000000000000 ) ) ;
#703 = VERTEX_POINT ( 'NONE', #9244 ) ;
#704 = ORIENTED_EDGE ( 'NONE', *, *, #4777, .T. ) ;
#705 = AXIS2_PLACEMENT_3D ( 'NONE', #1183, #466, #3392 ) ;
#706 = CARTESIAN_POINT ( 'NONE',  ( -53.29490495164537833, -48.67545040036925741, -60.28901569369804747 ) ) ;
#707 = PRODUCT_DEFINITION_SHAPE ( 'NONE', 'NONE',  #9476 ) ;
#708 = CARTESIAN_POINT ( 'NONE',  ( 4.000000000000000000, -7.653668647301985040, 17.72759065022987812 ) ) ;
#709 = EDGE_CURVE ( 'NONE', #4100, #933, #6475, .T. ) ;
#710 = VECTOR ( 'NONE', #3242, 1000.000000000000000 ) ;
#711 = EDGE_CURVE ( 'NONE', #2638, #8944, #9177, .T. ) ;
#712 = PLANE ( 'NONE',  #4815 ) ;
#713 = EDGE_CURVE ( 'NONE', #5539, #1940, #902, .T. ) ;
#714 = ADVANCED_FACE ( 'NONE', ( #4259 ), #9391, .T. ) ;
#715 = CARTESIAN_POINT ( 'NONE',  ( 22.50000000000000355, 0.000000000000000000, 2.000000000000035083 ) ) ;
#716 = ORIENTED_EDGE ( 'NONE', *, *, #2046, .F. ) ;
#717 = EDGE_LOOP ( 'NONE', ( #6670, #5208 ) ) ;
#718 = ORIENTED_EDGE ( 'NONE', *, *, #258, .T. ) ;
#719 = DIRECTION ( 'NONE',  ( -1.000000000000000000, 0.000000000000000000, 0.000000000000000000 ) ) ;
#720 = VERTEX_POINT ( 'NONE', #8674 ) ;
#721 = CIRCLE ( 'NONE', #4560, 15.00000000000000000 ) ;
#722 = CARTESIAN_POINT ( 'NONE',  ( -15.00000000000000000, 0.000000000000000000, 26.99999999999999289 ) ) ;
#723 = CARTESIAN_POINT ( 'NONE',  ( 0.000000000000000000, 0.000000000000000000, 0.000000000000000000 ) ) ;
#724 = VECTOR ( 'NONE', #985, 1000.000000000000000 ) ;
#725 = DIRECTION ( 'NONE',  ( -1.000000000000000000, -0.000000000000000000, -0.000000000000000000 ) ) ;
#726 = VECTOR ( 'NONE', #8362, 1000.000000000000000 ) ;
#727 = CARTESIAN_POINT ( 'NONE',  ( 27.00000000000000000, 43.00000000000000000, 11.99999999999999645 ) ) ;
#728 = EDGE_CURVE ( 'NONE', #4995, #5609, #7000, .T. ) ;
#729 = LINE ( 'NONE', #3662, #9036 ) ;
#730 = DIRECTION ( 'NONE',  ( -1.000000000000000000, 0.000000000000000000, 0.000000000000000000 ) ) ;
#731 = EDGE_CURVE ( 'NONE', #4380, #8166, #801, .T. ) ;
#732 = ORIENTED_EDGE ( 'NONE', *, *, #4518, .F. ) ;
#733 = CARTESIAN_POINT ( 'NONE',  ( 0.000000000000000000, 0.000000000000000000, 15.66147716702868209 ) ) ;
#734 = AXIS2_PLACEMENT_3D ( 'NONE', #7960, #4205, #1319 ) ;
#735 = ORIENTED_EDGE ( 'NONE', *, *, #8413, .T. ) ;
#736 = CYLINDRICAL_SURFACE ( 'NONE', #4488, 22.50000000000000000 ) ;
#737 = CARTESIAN_POINT ( 'NONE',  ( 32.00000000000000711, -34.99999999999999289, 5.000000000000004441 ) ) ;
#738 = DIRECTION ( 'NONE',  ( 0.000000000000000000, 0.000000000000000000, 1.000000000000000000 ) ) ;
#739 = DIRECTION ( 'NONE',  ( 0.000000000000000000, 0.000000000000000000, 1.000000000000000000 ) ) ;
#740 = EDGE_LOOP ( 'NONE', ( #5086, #9445 ) ) ;
#741 = EDGE_LOOP ( 'NONE', ( #8352, #2791, #1869, #1604 ) ) ;
#742 = DIRECTION ( 'NONE',  ( 0.000000000000000000, 0.000000000000000000, 1.000000000000000000 ) ) ;
#743 = ORIENTED_EDGE ( 'NONE', *, *, #6480, .T. ) ;
#744 = CARTESIAN_POINT ( 'NONE',  ( -25.50000000000000000, -7.855833012397050680E-14, 10.00000000000000000 ) ) ;
#745 = DIRECTION ( 'NONE',  ( 1.000000000000000000, 0.000000000000000000, 0.000000000000000000 ) ) ;
#746 = CIRCLE ( 'NONE', #4747, 3.000000000000002665 ) ;
#747 = LINE ( 'NONE', #3680, #3464 ) ;
#748 = AXIS2_PLACEMENT_3D ( 'NONE', #2990, #3859, #8037 ) ;
#749 = LINE ( 'NONE', #6766, #8751 ) ;
#750 = CARTESIAN_POINT ( 'NONE',  ( 0.000000000000000000, -18.47759065022712832, 8.403668647304948891 ) ) ;
#751 = CARTESIAN_POINT ( 'NONE',  ( -2.749999999999995559, 0.7500000000000000000, 1.500000000000000000 ) ) ;
#752 = CARTESIAN_POINT ( 'NONE',  ( -31.99999999999999289, -29.99999999999996447, 5.000000000000004441 ) ) ;
#753 = EDGE_CURVE ( 'NONE', #2323, #490, #5614, .T. ) ;
#754 = VERTEX_POINT ( 'NONE', #6293 ) ;
#755 = ORIENTED_EDGE ( 'NONE', *, *, #7404, .T. ) ;
#756 = FACE_OUTER_BOUND ( 'NONE', #328, .T. ) ;
#757 = CYLINDRICAL_SURFACE ( 'NONE', #4580, 3.000000000000002665 ) ;
#758 = EDGE_CURVE ( 'NONE', #2331, #2908, #463, .T. ) ;
#759 = CARTESIAN_POINT ( 'NONE',  ( -31.99999999999999289, -29.99999999999996447, 5.000000000000004441 ) ) ;
#760 = CARTESIAN_POINT ( 'NONE',  ( 0.7500000000000000000, 0.7500000000000000000, 1.500000000000000000 ) ) ;
#761 = DIRECTION ( 'NONE',  ( 0.000000000000000000, 0.000000000000000000, -1.000000000000000000 ) ) ;
#762 = ORIENTED_EDGE ( 'NONE', *, *, #5774, .F. ) ;
#763 = VERTEX_POINT ( 'NONE', #1956 ) ;
#764 = ORIENTED_EDGE ( 'NONE', *, *, #2101, .T. ) ;
#765 = DIRECTION ( 'NONE',  ( 0.9994148367277967404, 0.0008129226918946275224, 0.03419536935095436603 ) ) ;
#766 = ORIENTED_EDGE ( 'NONE', *, *, #4400, .F. ) ;
#767 = DIRECTION ( 'NONE',  ( -1.000000000000000000, 0.000000000000000000, 0.000000000000000000 ) ) ;
#768 = CARTESIAN_POINT ( 'NONE',  ( 0.7500000000000000000, 0.7500000000000000000, 1.500000000000000000 ) ) ;
#769 = LINE ( 'NONE', #3702, #4981 ) ;
#770 = PLANE ( 'NONE',  #2650 ) ;
#771 = FACE_OUTER_BOUND ( 'NONE', #4073, .T. ) ;
#772 = DIRECTION ( 'NONE',  ( -0.000000000000000000, -0.000000000000000000, -1.000000000000000000 ) ) ;
#773 = AXIS2_PLACEMENT_3D ( 'NONE', #2389, #939, #3871 ) ;
#774 = EDGE_CURVE ( 'NONE', #2124, #5549, #7816, .T. ) ;
#775 = ORIENTED_EDGE ( 'NONE', *, *, #3550, .T. ) ;
#776 = CARTESIAN_POINT ( 'NONE',  ( 2.749999999999996447, -0.7500000000000000000, 0.000000000000000000 ) ) ;
#777 = VERTEX_POINT ( 'NONE', #5071 ) ;
#778 = DIRECTION ( 'NONE',  ( 0.000000000000000000, 0.000000000000000000, -1.000000000000000000 ) ) ;
#779 = DIRECTION ( 'NONE',  ( 0.000000000000000000, 0.000000000000000000, 1.000000000000000000 ) ) ;
#780 = CARTESIAN_POINT ( 'NONE',  ( 0.000000000000000000, 0.000000000000000000, 5.000000000000000000 ) ) ;
#781 = DIRECTION ( 'NONE',  ( 1.000000000000000000, 0.000000000000000000, 0.000000000000000000 ) ) ;
#782 = AXIS2_PLACEMENT_3D ( 'NONE', #7082, #5747, #1994 ) ;
#783 = ORIENTED_EDGE ( 'NONE', *, *, #2600, .T. ) ;
#784 = ORIENTED_EDGE ( 'NONE', *, *, #3601, .F. ) ;
#785 = ORIENTED_EDGE ( 'NONE', *, *, #4032, .T. ) ;
#786 = CARTESIAN_POINT ( 'NONE',  ( 4.000000000000000000, -9.628187502531647418E-13, -19.99999999999950262 ) ) ;
#787 = CARTESIAN_POINT ( 'NONE',  ( 0.000000000000000000, 14.14213562373112154, -14.14213562373077870 ) ) ;
#788 = DIRECTION ( 'NONE',  ( -1.000000000000000000, 0.000000000000000000, -0.000000000000000000 ) ) ;
#789 = LINE ( 'NONE', #8960, #1229 ) ;
#790 = PLANE ( 'NONE',  #984 ) ;
#791 = CARTESIAN_POINT ( 'NONE',  ( 0.000000000000000000, -35.00000000000000000, 32.00000000000000000 ) ) ;
#792 = CARTESIAN_POINT ( 'NONE',  ( 5.000000000000000000, -18.47759065022790637, -7.653668647299759265 ) ) ;
#793 = ORIENTED_EDGE ( 'NONE', *, *, #7002, .F. ) ;
#794 = VERTEX_POINT ( 'NONE', #8808 ) ;
#795 = CARTESIAN_POINT ( 'NONE',  ( -27.00000000000000000, -43.00000000000000000, -25.00000000000000000 ) ) ;
#796 = CARTESIAN_POINT ( 'NONE',  ( -0.7500000000000000000, -0.7500000000000000000, 1.500000000000000000 ) ) ;
#797 = EDGE_LOOP ( 'NONE', ( #9401, #3064, #5815, #6633, #7802, #2283, #3467 ) ) ;
#798 = CONICAL_SURFACE ( 'NONE', #4334, 17.50000000000000355, 0.7853981633974533860 ) ;
#799 = CARTESIAN_POINT ( 'NONE',  ( -7.180166011355011868, 26.02777777777776436, 0.000000000000000000 ) ) ;
#800 = EDGE_CURVE ( 'NONE', #6840, #1397, #8148, .T. ) ;
#801 =( BOUNDED_CURVE ( )  B_SPLINE_CURVE ( 3, ( #4118, #3434, #4883, #1224 ),
 .UNSPECIFIED., .F., .T. ) 
 B_SPLINE_CURVE_WITH_KNOTS ( ( 4, 4 ),
 ( 3.213317012039606180, 4.712388980384689674 ),
 .UNSPECIFIED. ) 
 CURVE ( )  GEOMETRIC_REPRESENTATION_ITEM ( )  RATIONAL_B_SPLINE_CURVE ( ( 1.000000000000000000, 0.8213367208436765932, 0.8213367208436765932, 1.000000000000000000 ) ) 
 REPRESENTATION_ITEM ( '' )  );
#802 = DIRECTION ( 'NONE',  ( 0.5773502691896252870, -0.5773502691896258421, -0.5773502691896261751 ) ) ;
#803 = FACE_OUTER_BOUND ( 'NONE', #3328, .T. ) ;
#804 = VERTEX_POINT ( 'NONE', #2228 ) ;
#805 = EDGE_CURVE ( 'NONE', #6613, #5515, #7492, .T. ) ;
#806 = ORIENTED_EDGE ( 'NONE', *, *, #8639, .T. ) ;
#807 = CIRCLE ( 'NONE', #357, 22.00000000000000711 ) ;
#808 = DIRECTION ( 'NONE',  ( -1.109981221398774256E-16, -0.9911323735125173728, 0.1328782080532535381 ) ) ;
#809 = DIRECTION ( 'NONE',  ( -0.000000000000000000, -0.000000000000000000, -1.000000000000000000 ) ) ;
#810 = DIRECTION ( 'NONE',  ( -1.000000000000000000, 0.000000000000000000, 0.000000000000000000 ) ) ;
#811 = CARTESIAN_POINT ( 'NONE',  ( 0.000000000000000000, -20.00000000000120437, -1.559999999999665432 ) ) ;
#812 = VECTOR ( 'NONE', #8914, 1000.000000000000000 ) ;
#813 = CARTESIAN_POINT ( 'NONE',  ( 4.000000000000000000, -20.00000000000120437, -1.559999999999665432 ) ) ;
#814 = EDGE_CURVE ( 'NONE', #1024, #7251, #8573, .T. ) ;
#815 = FACE_OUTER_BOUND ( 'NONE', #6771, .T. ) ;
#816 = DIRECTION ( 'NONE',  ( 1.000000000000000000, -0.000000000000000000, -0.000000000000000000 ) ) ;
#817 = ORIENTED_EDGE ( 'NONE', *, *, #7545, .F. ) ;
#818 = LINE ( 'NONE', #922, #8704 ) ;
#819 = ORIENTED_EDGE ( 'NONE', *, *, #104, .F. ) ;
#820 = CARTESIAN_POINT ( 'NONE',  ( 1.571166602479410136E-13, -22.50000000000000355, 0.000000000000000000 ) ) ;
#821 = CARTESIAN_POINT ( 'NONE',  ( 37.00000000000000000, -15.90990257669733943, -57.09009742330271564 ) ) ;
#823 = EDGE_CURVE ( 'NONE', #8944, #2638, #9332, .T. ) ;
#822 = LINE ( 'NONE', #3762, #9334 ) ;
#824 = ADVANCED_FACE ( 'NONE', ( #76 ), #3055, .F. ) ;
#825 = AXIS2_PLACEMENT_3D ( 'NONE', #1228, #9202, #9397 ) ;
#826 = FACE_OUTER_BOUND ( 'NONE', #3541, .T. ) ;
#827 = EDGE_LOOP ( 'NONE', ( #4902, #309, #5550, #5021 ) ) ;
#828 = AXIS2_PLACEMENT_3D ( 'NONE', #5412, #7671, #8527 ) ;
#829 = EDGE_CURVE ( 'NONE', #6912, #2947, #5199, .T. ) ;
#830 = EDGE_CURVE ( 'NONE', #75, #6840, #1791, .T. ) ;
#831 = ORIENTED_EDGE ( 'NONE', *, *, #3103, .T. ) ;
#832 = ORIENTED_EDGE ( 'NONE', *, *, #4823, .T. ) ;
#833 =( NAMED_UNIT ( * ) PLANE_ANGLE_UNIT ( ) SI_UNIT ( $, .RADIAN. ) );
#834 = ORIENTED_EDGE ( 'NONE', *, *, #6458, .T. ) ;
#835 = LINE ( 'NONE', #3769, #2450 ) ;
#836 = DIRECTION ( 'NONE',  ( -1.000000000000000000, -0.000000000000000000, -0.000000000000000000 ) ) ;
#837 = CARTESIAN_POINT ( 'NONE',  ( 37.00000000000000000, -15.90990257669733943, -54.09009742330271564 ) ) ;
#838 = CONICAL_SURFACE ( 'NONE', #2540, 6.000000000000000888, 0.7853981633974498333 ) ;
#839 = FACE_OUTER_BOUND ( 'NONE', #4855, .T. ) ;
#840 = DIRECTION ( 'NONE',  ( 0.000000000000000000, 0.000000000000000000, 1.000000000000000000 ) ) ;
#841 = EDGE_CURVE ( 'NONE', #3430, #5108, #5965, .T. ) ;
#842 = FACE_OUTER_BOUND ( 'NONE', #1082, .T. ) ;
#843 = CYLINDRICAL_SURFACE ( 'NONE', #2052, 2.999999999999999556 ) ;
#844 = EDGE_CURVE ( 'NONE', #2915, #287, #5888, .T. ) ;
#845 = ORIENTED_EDGE ( 'NONE', *, *, #6602, .T. ) ;
#846 = ORIENTED_EDGE ( 'NONE', *, *, #9070, .T. ) ;
#847 = EDGE_CURVE ( 'NONE', #2113, #8405, #2894, .T. ) ;
#848 = LINE ( 'NONE', #1473, #9157 ) ;
#849 = VERTEX_POINT ( 'NONE', #7325 ) ;
#850 = ORIENTED_EDGE ( 'NONE', *, *, #8658, .F. ) ;
#851 = CARTESIAN_POINT ( 'NONE',  ( -6.186958832529963814, 26.79406326810229189, 0.4926121009229034176 ) ) ;
#852 = CARTESIAN_POINT ( 'NONE',  ( 4.000000000000000000, -7.653668647301985040, 19.22759065022772873 ) ) ;
#853 = PRODUCT_DEFINITION_CONTEXT ( 'detailed design', #8359, 'design' ) ;
#854 = CARTESIAN_POINT ( 'NONE',  ( 60.00000000000000000, -12.50000000000000000, -100.0000000000000000 ) ) ;
#855 = AXIS2_PLACEMENT_3D ( 'NONE', #607, #9439, #1415 ) ;
#856 = ORIENTED_EDGE ( 'NONE', *, *, #2427, .F. ) ;
#857 = ORIENTED_EDGE ( 'NONE', *, *, #4299, .T. ) ;
#858 = APPLICATION_PROTOCOL_DEFINITION ( 'draft international standard', 'automotive_design', 1998, #1792 ) ;
#859 = CYLINDRICAL_SURFACE ( 'NONE', #2232, 11.00000000000000000 ) ;
#860 = CARTESIAN_POINT ( 'NONE',  ( 16.50000000000000000, 0.000000000000000000, 2.000000000000035083 ) ) ;
#861 = AXIS2_PLACEMENT_3D ( 'NONE', #9190, #3916, #1078 ) ;
#862 = AXIS2_PLACEMENT_3D ( 'NONE', #5379, #2493, #7676 ) ;
#863 = DIRECTION ( 'NONE',  ( 0.000000000000000000, 0.000000000000000000, -1.000000000000000000 ) ) ;
#864 = PRODUCT_DEFINITION_SHAPE ( 'NONE', 'NONE',  #9484 ) ;
#865 = CARTESIAN_POINT ( 'NONE',  ( 60.00000000000000000, -15.90990257669733943, -54.09009742330271564 ) ) ;
#866 = LINE ( 'NONE', #6548, #148 ) ;
#867 = DIRECTION ( 'NONE',  ( 0.000000000000000000, 1.000000000000000000, 0.000000000000000000 ) ) ;
#868 = DIRECTION ( 'NONE',  ( -0.000000000000000000, -0.000000000000000000, -1.000000000000000000 ) ) ;
#869 = AXIS2_PLACEMENT_3D ( 'NONE', #2272, #7890, #5920 ) ;
#870 = ORIENTED_EDGE ( 'NONE', *, *, #6924, .F. ) ;
#871 = CIRCLE ( 'NONE', #7781, 6.000000000000001776 ) ;
#872 = ORIENTED_EDGE ( 'NONE', *, *, #5714, .F. ) ;
#873 = VECTOR ( 'NONE', #816, 1000.000000000000000 ) ;
#874 = DIRECTION ( 'NONE',  ( -1.000000000000000000, 0.000000000000000000, 0.000000000000000000 ) ) ;
#875 = CYLINDRICAL_SURFACE ( 'NONE', #2570, 0.7499999999982936982 ) ;
#876 = AXIS2_PLACEMENT_3D ( 'NONE', #3595, #3018, #2251 ) ;
#877 = PRESENTATION_LAYER_ASSIGNMENT (  '', '', ( #2424 ) ) ;
#878 = DIRECTION ( 'NONE',  ( 0.000000000000000000, 1.000000000000000000, 0.000000000000000000 ) ) ;
#879 = VECTOR ( 'NONE', #1538, 1000.000000000000000 ) ;
#880 = CARTESIAN_POINT ( 'NONE',  ( -3.500000000000000000, 2.818925648462311528E-15, 0.000000000000000000 ) ) ;
#881 = VECTOR ( 'NONE', #2152, 1000.000000000000000 ) ;
#882 = ORIENTED_EDGE ( 'NONE', *, *, #4636, .F. ) ;
#883 = VERTEX_POINT ( 'NONE', #744 ) ;
#884 = AXIS2_PLACEMENT_3D ( 'NONE', #8973, #2356, #3934 ) ;
#885 = ORIENTED_EDGE ( 'NONE', *, *, #3309, .F. ) ;
#886 = ORIENTED_EDGE ( 'NONE', *, *, #3534, .F. ) ;
#887 = AXIS2_PLACEMENT_3D ( 'NONE', #3361, #3310, #9168 ) ;
#888 = DIRECTION ( 'NONE',  ( -1.000000000000000000, 0.000000000000000000, 0.000000000000000000 ) ) ;
#889 = EDGE_CURVE ( 'NONE', #3554, #2688, #4126, .T. ) ;
#890 = CARTESIAN_POINT ( 'NONE',  ( 30.00000000000000000, 0.000000000000000000, 3.000000000000052847 ) ) ;
#891 = CARTESIAN_POINT ( 'NONE',  ( 0.7500000000000000000, 0.7500000000000000000, 1.500000000000000000 ) ) ;
#892 = EDGE_CURVE ( 'NONE', #6251, #3861, #7658, .T. ) ;
#893 = CIRCLE ( 'NONE', #9021, 7.250000000000002665 ) ;
#894 = EDGE_CURVE ( 'NONE', #1738, #8284, #835, .T. ) ;
#895 = EDGE_CURVE ( 'NONE', #4382, #1673, #652, .T. ) ;
#896 = LINE ( 'NONE', #3824, #3532 ) ;
#897 = DIRECTION ( 'NONE',  ( -1.000000000000000000, 0.000000000000000000, 0.000000000000000000 ) ) ;
#898 = SURFACE_SIDE_STYLE ('',( #6808 ) ) ;
#899 = CARTESIAN_POINT ( 'NONE',  ( 27.00000000000000000, -43.00000000000000000, 11.99999999999999645 ) ) ;
#900 = VERTEX_POINT ( 'NONE', #127 ) ;
#901 = ORIENTED_EDGE ( 'NONE', *, *, #8588, .T. ) ;
#902 = CIRCLE ( 'NONE', #3664, 3.000000000000000000 ) ;
#903 = LINE ( 'NONE', #4459, #5794 ) ;
#904 = ORIENTED_EDGE ( 'NONE', *, *, #5117, .F. ) ;
#905 = LINE ( 'NONE', #3836, #422 ) ;
#906 = TOROIDAL_SURFACE ( 'NONE', #4897, 5.000000000000000888, 1.000000000000000000 ) ;
#907 = EDGE_CURVE ( 'NONE', #6587, #7179, #5822, .T. ) ;
#908 = DIRECTION ( 'NONE',  ( 0.000000000000000000, 0.000000000000000000, 1.000000000000000000 ) ) ;
#909 = CARTESIAN_POINT ( 'NONE',  ( 17.50000000000000355, 0.000000000000000000, 14.49999999999999822 ) ) ;
#910 = ORIENTED_EDGE ( 'NONE', *, *, #3003, .F. ) ;
#911 = ORIENTED_EDGE ( 'NONE', *, *, #8809, .F. ) ;
#912 = SHAPE_DEFINITION_REPRESENTATION ( #7841, #8501 ) ;
#913 = EDGE_CURVE ( 'NONE', #1970, #4478, #7805, .T. ) ;
#914 = CARTESIAN_POINT ( 'NONE',  ( 0.000000000000000000, 0.000000000000000000, 3.000000000000052847 ) ) ;
#915 = DIRECTION ( 'NONE',  ( -0.000000000000000000, 1.000000000000000000, 0.000000000000000000 ) ) ;
#916 = CARTESIAN_POINT ( 'NONE',  ( -3.000000000000000444, 0.000000000000000000, 5.000000000000000000 ) ) ;
#917 = FACE_OUTER_BOUND ( 'NONE', #7223, .T. ) ;
#918 = FACE_OUTER_BOUND ( 'NONE', #5596, .T. ) ;
#919 = DIRECTION ( 'NONE',  ( 0.000000000000000000, 0.000000000000000000, 1.000000000000000000 ) ) ;
#920 = CARTESIAN_POINT ( 'NONE',  ( 0.4367635713303894551, -28.48785780768278286, 1.490418226835889426 ) ) ;
#921 = ORIENTED_EDGE ( 'NONE', *, *, #3528, .F. ) ;
#922 = CARTESIAN_POINT ( 'NONE',  ( 60.00000000000000000, -15.90990257669733943, -88.90990257669730568 ) ) ;
#923 = ORIENTED_EDGE ( 'NONE', *, *, #5717, .F. ) ;
#924 = DIRECTION ( 'NONE',  ( 0.000000000000000000, 0.000000000000000000, -1.000000000000000000 ) ) ;
#925 = DIRECTION ( 'NONE',  ( 0.000000000000000000, 0.000000000000000000, 1.000000000000000000 ) ) ;
#926 = DIRECTION ( 'NONE',  ( -0.000000000000000000, -0.000000000000000000, -1.000000000000000000 ) ) ;
#927 = ADVANCED_FACE ( 'NONE', ( #6803 ), #8330, .F. ) ;
#928 = CARTESIAN_POINT ( 'NONE',  ( 0.000000000000000000, 14.14213562373247868, 15.70213562373191962 ) ) ;
#929 = AXIS2_PLACEMENT_3D ( 'NONE', #1666, #4598, #1516 ) ;
#930 = ORIENTED_EDGE ( 'NONE', *, *, #2550, .T. ) ;
#931 = ORIENTED_EDGE ( 'NONE', *, *, #8715, .T. ) ;
#932 = EDGE_CURVE ( 'NONE', #3514, #2323, #9167, .T. ) ;
#933 = VERTEX_POINT ( 'NONE', #1749 ) ;
#934 = ORIENTED_EDGE ( 'NONE', *, *, #1402, .F. ) ;
#935 = DIRECTION ( 'NONE',  ( -1.000000000000000000, 0.000000000000000000, 0.000000000000000000 ) ) ;
#936 = CARTESIAN_POINT ( 'NONE',  ( 53.29490495164537833, -3.673940397442057600E-15, -70.00000000000000000 ) ) ;
#937 = VECTOR ( 'NONE', #455, 999.9999999999998863 ) ;
#938 = FACE_OUTER_BOUND ( 'NONE', #5383, .T. ) ;
#939 = DIRECTION ( 'NONE',  ( 0.000000000000000000, 0.000000000000000000, -1.000000000000000000 ) ) ;
#940 = CARTESIAN_POINT ( 'NONE',  ( 3.000000000000000000, -22.50000000000000355, 5.000000000000000000 ) ) ;
#941 = DIRECTION ( 'NONE',  ( 0.7071067811865450192, -0.5000000000000019984, 0.5000000000000016653 ) ) ;
#942 = DIRECTION ( 'NONE',  ( 1.000000000000000000, 0.000000000000000000, 0.000000000000000000 ) ) ;
#943 = VERTEX_POINT ( 'NONE', #8191 ) ;
#944 = ORIENTED_EDGE ( 'NONE', *, *, #2603, .T. ) ;
#945 = FACE_OUTER_BOUND ( 'NONE', #6900, .T. ) ;
#946 = EDGE_LOOP ( 'NONE', ( #4686, #3454, #2994, #6192 ) ) ;
#947 = FACE_OUTER_BOUND ( 'NONE', #6280, .T. ) ;
#948 = ORIENTED_EDGE ( 'NONE', *, *, #1475, .T. ) ;
#949 = DIRECTION ( 'NONE',  ( -1.000000000000000000, -0.000000000000000000, -0.000000000000000000 ) ) ;
#950 = EDGE_CURVE ( 'NONE', #8301, #4792, #3047, .T. ) ;
#951 =( BOUNDED_CURVE ( )  B_SPLINE_CURVE ( 3, ( #8151, #3772, #8047, #1564 ),
 .UNSPECIFIED., .F., .F. ) 
 B_SPLINE_CURVE_WITH_KNOTS ( ( 4, 4 ),
 ( 5.805906910357376383, 6.283185307179586232 ),
 .UNSPECIFIED. ) 
 CURVE ( )  GEOMETRIC_REPRESENTATION_ITEM ( )  RATIONAL_B_SPLINE_CURVE ( ( 1.000000000000000000, 0.9811070276743185659, 0.9811070276743185659, 1.000000000000000000 ) ) 
 REPRESENTATION_ITEM ( '' )  );
#952 = EDGE_CURVE ( 'NONE', #3120, #5090, #746, .T. ) ;
#953 = DIRECTION ( 'NONE',  ( 1.000000000000000000, -0.000000000000000000, -0.000000000000000000 ) ) ;
#954 = CARTESIAN_POINT ( 'NONE',  ( -2.323800269068097446, -28.49052126930483197, 1.583192244553113914 ) ) ;
#955 = VERTEX_POINT ( 'NONE', #175 ) ;
#956 = VERTEX_POINT ( 'NONE', #1660 ) ;
#957 = AXIS2_PLACEMENT_3D ( 'NONE', #5381, #8341, #1764 ) ;
#958 =( NAMED_UNIT ( * ) PLANE_ANGLE_UNIT ( ) SI_UNIT ( $, .RADIAN. ) );
#959 = VECTOR ( 'NONE', #9416, 1000.000000000000000 ) ;
#960 = DIRECTION ( 'NONE',  ( -0.000000000000000000, -0.000000000000000000, -1.000000000000000000 ) ) ;
#961 = DIRECTION ( 'NONE',  ( -1.000000000000000000, 0.000000000000000000, -0.000000000000000000 ) ) ;
#962 = CARTESIAN_POINT ( 'NONE',  ( -60.00000000000000000, 30.00000000000000000, -13.00000000000000000 ) ) ;
#963 = DIRECTION ( 'NONE',  ( -1.000000000000000000, 0.000000000000000000, 0.000000000000000000 ) ) ;
#964 = VECTOR ( 'NONE', #2804, 1000.000000000000000 ) ;
#965 = FACE_OUTER_BOUND ( 'NONE', #8996, .T. ) ;
#966 = DIRECTION ( 'NONE',  ( -1.000000000000000000, 0.000000000000000000, 0.000000000000000000 ) ) ;
#967 = ORIENTED_EDGE ( 'NONE', *, *, #4663, .T. ) ;
#968 = SURFACE_STYLE_FILL_AREA ( #108 ) ;
#969 = ORIENTED_EDGE ( 'NONE', *, *, #1072, .F. ) ;
#970 = LINE ( 'NONE', #6793, #5257 ) ;
#971 = DIRECTION ( 'NONE',  ( 0.000000000000000000, 0.000000000000000000, -1.000000000000000000 ) ) ;
#972 = AXIS2_PLACEMENT_3D ( 'NONE', #1152, #1063, #8364 ) ;
#973 = LINE ( 'NONE', #3323, #1059 ) ;
#974 = CARTESIAN_POINT ( 'NONE',  ( -38.00000000000000711, -44.39318849903268926, -6.762951650419163130 ) ) ;
#975 = VERTEX_POINT ( 'NONE', #1029 ) ;
#976 = ORIENTED_EDGE ( 'NONE', *, *, #3071, .T. ) ;
#977 = ORIENTED_EDGE ( 'NONE', *, *, #758, .F. ) ;
#978 = ORIENTED_EDGE ( 'NONE', *, *, #1905, .F. ) ;
#979 = CARTESIAN_POINT ( 'NONE',  ( 60.00000000000001421, -9.637301612213114765, -29.99999999999998934 ) ) ;
#980 = CARTESIAN_POINT ( 'NONE',  ( 27.00000000000000355, 0.000000000000000000, 64.00000000000000000 ) ) ;
#981 = FACE_OUTER_BOUND ( 'NONE', #4924, .T. ) ;
#982 = VECTOR ( 'NONE', #3353, 1000.000000000000000 ) ;
#983 = DIRECTION ( 'NONE',  ( 0.2588190451025176309, 3.169619151431726731E-17, -0.9659258262890692004 ) ) ;
#984 = AXIS2_PLACEMENT_3D ( 'NONE', #2233, #6767, #6857 ) ;
#985 = DIRECTION ( 'NONE',  ( -0.000000000000000000, -0.000000000000000000, -1.000000000000000000 ) ) ;
#986 = FACE_OUTER_BOUND ( 'NONE', #5203, .T. ) ;
#987 = ORIENTED_EDGE ( 'NONE', *, *, #6818, .F. ) ;
#988 = CIRCLE ( 'NONE', #6517, 6.000000000000001776 ) ;
#989 = EDGE_LOOP ( 'NONE', ( #1864, #1558 ) ) ;
#990 = DIRECTION ( 'NONE',  ( 0.000000000000000000, 0.000000000000000000, 1.000000000000000000 ) ) ;
#991 = VERTEX_POINT ( 'NONE', #4541 ) ;
#992 = FACE_OUTER_BOUND ( 'NONE', #9110, .T. ) ;
#993 = DIRECTION ( 'NONE',  ( -1.000000000000000000, 0.000000000000000000, 0.000000000000000000 ) ) ;
#994 = CIRCLE ( 'NONE', #6372, 26.99999999999999645 ) ;
#995 = ORIENTED_EDGE ( 'NONE', *, *, #2557, .F. ) ;
#996 = APPLICATION_CONTEXT ( 'automotive_design' ) ;
#997 = CYLINDRICAL_SURFACE ( 'NONE', #9161, 3.000000000000002665 ) ;
#998 = FACE_BOUND ( 'NONE', #1821, .T. ) ;
#999 = CYLINDRICAL_SURFACE ( 'NONE', #5801, 3.000000000000002665 ) ;
#1000 = VERTEX_POINT ( 'NONE', #4592 ) ;
#1001 = EDGE_LOOP ( 'NONE', ( #5875, #1692, #2814, #3013 ) ) ;
#1002 = PRODUCT_DEFINITION_FORMATION_WITH_SPECIFIED_SOURCE ( 'ANY', '', #9448, .NOT_KNOWN. ) ;
#1003 = ITEM_DEFINED_TRANSFORMATION ( 'NONE', 'NONE', #7138,  #1614 ) ;
#1004 = EDGE_CURVE ( 'NONE', #4533, #1970, #8239, .T. ) ;
#1005 =( BOUNDED_CURVE ( )  B_SPLINE_CURVE ( 3, ( #543, #9331, #4964, #1942 ),
 .UNSPECIFIED., .F., .F. ) 
 B_SPLINE_CURVE_WITH_KNOTS ( ( 4, 4 ),
 ( 3.141592653589793116, 3.926990816987241395 ),
 .UNSPECIFIED. ) 
 CURVE ( )  GEOMETRIC_REPRESENTATION_ITEM ( )  RATIONAL_B_SPLINE_CURVE ( ( 1.000000000000000000, 0.9492530216741911220, 0.9492530216741911220, 1.000000000000000000 ) ) 
 REPRESENTATION_ITEM ( '' )  );
#1006 = DIRECTION ( 'NONE',  ( 1.000000000000000000, 0.000000000000000000, 0.000000000000000000 ) ) ;
#1007 = EDGE_CURVE ( 'NONE', #6890, #1286, #5367, .T. ) ;
#1008 = EDGE_CURVE ( 'NONE', #5740, #5476, #5509, .T. ) ;
#1009 = EDGE_CURVE ( 'NONE', #301, #8237, #3646, .T. ) ;
#1010 = FACE_OUTER_BOUND ( 'NONE', #6789, .T. ) ;
#1011 =( LENGTH_UNIT ( ) NAMED_UNIT ( * ) SI_UNIT ( .MILLI., .METRE. ) );
#1012 = CARTESIAN_POINT ( 'NONE',  ( 0.7500000000000000000, 2.749999999999995559, 1.500000000000000000 ) ) ;
#1013 = CARTESIAN_POINT ( 'NONE',  ( -27.86926932341927809, 4.210987672173478025, 1.183815993626686991 ) ) ;
#1014 = ORIENTED_EDGE ( 'NONE', *, *, #2234, .T. ) ;
#1015 = DIRECTION ( 'NONE',  ( -1.000000000000000000, 0.000000000000000000, 0.000000000000000000 ) ) ;
#1016 = ORIENTED_EDGE ( 'NONE', *, *, #435, .T. ) ;
#1017 = VECTOR ( 'NONE', #6765, 1000.000000000000000 ) ;
#1018 = PLANE ( 'NONE',  #1104 ) ;
#1019 = DIRECTION ( 'NONE',  ( 0.000000000000000000, -1.000000000000000000, 0.000000000000000000 ) ) ;
#1020 = DIRECTION ( 'NONE',  ( 1.000000000000000000, 0.000000000000000000, 0.000000000000000000 ) ) ;
#1021 = CARTESIAN_POINT ( 'NONE',  ( -37.73845885098650399, -45.76160744848117190, -6.169970105658154402 ) ) ;
#1022 = AXIS2_PLACEMENT_3D ( 'NONE', #7357, #1546, #3901 ) ;
#1023 = EDGE_CURVE ( 'NONE', #8436, #8187, #4586, .T. ) ;
#1024 = VERTEX_POINT ( 'NONE', #3238 ) ;
#1025 = ORIENTED_EDGE ( 'NONE', *, *, #5159, .F. ) ;
#1026 = ORIENTED_EDGE ( 'NONE', *, *, #4417, .T. ) ;
#1027 = ORIENTED_EDGE ( 'NONE', *, *, #7993, .T. ) ;
#1028 = CIRCLE ( 'NONE', #4104, 15.00000000000000000 ) ;
#1029 = CARTESIAN_POINT ( 'NONE',  ( 60.00000000000000000, 7.347880794884118356E-15, 23.99999999999998579 ) ) ;
#1030 = DIRECTION ( 'NONE',  ( 0.000000000000000000, -0.000000000000000000, 1.000000000000000000 ) ) ;
#1031 = EDGE_CURVE ( 'NONE', #4623, #5090, #6140, .T. ) ;
#1032 = CIRCLE ( 'NONE', #3186, 6.000000000000000888 ) ;
#1033 = LINE ( 'NONE', #5507, #1636 ) ;
#1034 = CIRCLE ( 'NONE', #7314, 2.999999999999999112 ) ;
#1035 = DIRECTION ( 'NONE',  ( 0.000000000000000000, 0.000000000000000000, 1.000000000000000000 ) ) ;
#1036 = AXIS2_PLACEMENT_3D ( 'NONE', #5375, #941, #7472 ) ;
#1037 = AXIS2_PLACEMENT_3D ( 'NONE', #792, #84, #5222 ) ;
#1038 = AXIS2_PLACEMENT_3D ( 'NONE', #8823, #5176, #4791 ) ;
#1039 = FACE_OUTER_BOUND ( 'NONE', #3301, .T. ) ;
#1040 = ORIENTED_EDGE ( 'NONE', *, *, #1125, .F. ) ;
#1041 = VERTEX_POINT ( 'NONE', #6086 ) ;
#1042 = FACE_OUTER_BOUND ( 'NONE', #4857, .T. ) ;
#1043 = EDGE_LOOP ( 'NONE', ( #4538, #3271, #886 ) ) ;
#1044 = DIRECTION ( 'NONE',  ( -0.7071067811865444641, 0.7071067811865505703, 0.000000000000000000 ) ) ;
#1045 = LINE ( 'NONE', #6153, #3192 ) ;
#1046 =( GEOMETRIC_REPRESENTATION_CONTEXT ( 3 ) GLOBAL_UNCERTAINTY_ASSIGNED_CONTEXT ( ( #2403 ) ) GLOBAL_UNIT_ASSIGNED_CONTEXT ( ( #1011, #6067, #4619 ) ) REPRESENTATION_CONTEXT ( 'NONE', 'WORKASPACE' ) );
#1047 = ORIENTED_EDGE ( 'NONE', *, *, #1240, .F. ) ;
#1048 = CARTESIAN_POINT ( 'NONE',  ( 0.7500000000000000000, 0.7500000000000000000, 0.000000000000000000 ) ) ;
#1049 = EDGE_CURVE ( 'NONE', #3283, #8519, #7962, .T. ) ;
#1050 = PLANE ( 'NONE',  #5443 ) ;
#1051 = CARTESIAN_POINT ( 'NONE',  ( -4.208878922505766340, -27.87018698802495464, 1.184405920873192075 ) ) ;
#1052 = ORIENTED_EDGE ( 'NONE', *, *, #5118, .T. ) ;
#1053 = AXIS2_PLACEMENT_3D ( 'NONE', #5638, #7795, #1348 ) ;
#1054 = ORIENTED_EDGE ( 'NONE', *, *, #4209, .T. ) ;
#1055 = EDGE_CURVE ( 'NONE', #8953, #9116, #866, .T. ) ;
#1056 = PRODUCT_CONTEXT ( 'NONE', #6585, 'mechanical' ) ;
#1057 = VECTOR ( 'NONE', #5268, 1000.000000000000000 ) ;
#1058 = CARTESIAN_POINT ( 'NONE',  ( 0.000000000000000000, 29.99999999999997158, 64.00000000000000000 ) ) ;
#1059 = VECTOR ( 'NONE', #7701, 1000.000000000000000 ) ;
#1060 = DIRECTION ( 'NONE',  ( -1.000000000000000000, 0.000000000000000000, -0.000000000000000000 ) ) ;
#1061 = DIRECTION ( 'NONE',  ( -1.000000000000000000, 0.000000000000000000, 0.000000000000000000 ) ) ;
#1062 = DIRECTION ( 'NONE',  ( 1.000000000000000000, 0.000000000000000000, 0.000000000000000000 ) ) ;
#1063 = DIRECTION ( 'NONE',  ( 0.000000000000000000, 0.000000000000000000, -1.000000000000000000 ) ) ;
#1064 = ORIENTED_EDGE ( 'NONE', *, *, #6422, .T. ) ;
#1065 = CARTESIAN_POINT ( 'NONE',  ( 0.000000000000000000, -9.626277053524975217E-13, -21.56000000000076966 ) ) ;
#1066 = ORIENTED_EDGE ( 'NONE', *, *, #7565, .F. ) ;
#1067 = DIRECTION ( 'NONE',  ( 0.000000000000000000, 0.000000000000000000, -1.000000000000000000 ) ) ;
#1068 = CARTESIAN_POINT ( 'NONE',  ( 4.000000000000000000, 20.00000000000120437, 7.412591687719288072E-13 ) ) ;
#1069 = PLANE ( 'NONE',  #2288 ) ;
#1070 = CIRCLE ( 'NONE', #162, 7.250000000000002665 ) ;
#1071 = CARTESIAN_POINT ( 'NONE',  ( 43.18827341296427846, -42.33902489539482161, -7.653089211995572683 ) ) ;
#1072 = EDGE_CURVE ( 'NONE', #6494, #1522, #8028, .T. ) ;
#1073 = EDGE_LOOP ( 'NONE', ( #3291, #1027, #5277, #3734 ) ) ;
#1074 = ORIENTED_EDGE ( 'NONE', *, *, #2810, .F. ) ;
#1075 = ORIENTED_EDGE ( 'NONE', *, *, #1004, .F. ) ;
#1076 = VERTEX_POINT ( 'NONE', #4519 ) ;
#1077 = LINE ( 'NONE', #6141, #5103 ) ;
#1078 = DIRECTION ( 'NONE',  ( 0.000000000000000000, 0.000000000000000000, 1.000000000000000000 ) ) ;
#1079 = AXIS2_PLACEMENT_3D ( 'NONE', #1419, #8677, #509 ) ;
#1080 = CARTESIAN_POINT ( 'NONE',  ( 40.05867498135629745, -15.23141075423630575, -98.05867498135631877 ) ) ;
#1081 = CARTESIAN_POINT ( 'NONE',  ( 27.16400976452047189, 3.794195651236313083, 0.4256031388450388087 ) ) ;
#1082 = EDGE_LOOP ( 'NONE', ( #2203, #6488, #5793, #3396, #2394, #6109 ) ) ;
#1083 = ORIENTED_EDGE ( 'NONE', *, *, #2430, .T. ) ;
#1084 = DIRECTION ( 'NONE',  ( 0.000000000000000000, 0.000000000000000000, -1.000000000000000000 ) ) ;
#1085 = ORIENTED_EDGE ( 'NONE', *, *, #4803, .F. ) ;
#1086 = FACE_OUTER_BOUND ( 'NONE', #9186, .T. ) ;
#1087 = ORIENTED_EDGE ( 'NONE', *, *, #3711, .F. ) ;
#1088 = DIRECTION ( 'NONE',  ( -1.000000000000000000, 0.000000000000000000, 0.000000000000000000 ) ) ;
#1089 = CARTESIAN_POINT ( 'NONE',  ( 52.42476942962458963, -29.19763577280656008, -80.99738777760515518 ) ) ;
#1090 = LINE ( 'NONE', #4611, #8857 ) ;
#1091 = ORIENTED_EDGE ( 'NONE', *, *, #1126, .T. ) ;
#1092 = EDGE_LOOP ( 'NONE', ( #2816, #8479 ) ) ;
#1093 = CIRCLE ( 'NONE', #5560, 13.66147716702868031 ) ;
#1094 = CONTEXT_DEPENDENT_SHAPE_REPRESENTATION ( #9031, #5003 ) ;
#1095 = EDGE_CURVE ( 'NONE', #6009, #3216, #4282, .T. ) ;
#1096 = CARTESIAN_POINT ( 'NONE',  ( -2.749999999999995559, 0.7500000000000000000, 0.000000000000000000 ) ) ;
#1097 = ADVANCED_FACE ( 'NONE', ( #678, #4378 ), #8749, .T. ) ;
#1098 = CIRCLE ( 'NONE', #196, 59.00000000000000000 ) ;
#1099 = CARTESIAN_POINT ( 'NONE',  ( -51.96152422706632734, 30.00000000000000000, -80.85015119857381194 ) ) ;
#1100 = ADVANCED_FACE ( 'NONE', ( #771 ), #5823, .F. ) ;
#1101 = CARTESIAN_POINT ( 'NONE',  ( -39.50000000000000711, -14.99999999999999289, -97.50000000000001421 ) ) ;
#1102 = CYLINDRICAL_SURFACE ( 'NONE', #1185, 0.7500000000000015543 ) ;
#1103 = CARTESIAN_POINT ( 'NONE',  ( 2.750000000000006661, 0.7500000000000000000, 1.500000000000000000 ) ) ;
#1104 = AXIS2_PLACEMENT_3D ( 'NONE', #303, #8278, #3956 ) ;
#1105 = ORIENTED_EDGE ( 'NONE', *, *, #841, .T. ) ;
#1106 = LINE ( 'NONE', #2561, #7473 ) ;
#1107 = VERTEX_POINT ( 'NONE', #3705 ) ;
#1108 = DIRECTION ( 'NONE',  ( 0.000000000000000000, 0.000000000000000000, 1.000000000000000000 ) ) ;
#1109 = DIRECTION ( 'NONE',  ( 1.000000000000000000, 0.000000000000000000, 0.000000000000000000 ) ) ;
#1110 = AXIS2_PLACEMENT_3D ( 'NONE', #400, #4914, #453 ) ;
#1111 = EDGE_CURVE ( 'NONE', #3876, #7733, #7502, .T. ) ;
#1112 = DIRECTION ( 'NONE',  ( 1.000000000000000000, 0.000000000000000000, 0.000000000000000000 ) ) ;
#1113 = FACE_OUTER_BOUND ( 'NONE', #6047, .T. ) ;
#1114 = ORIENTED_EDGE ( 'NONE', *, *, #4456, .T. ) ;
#1115 = VERTEX_POINT ( 'NONE', #1542 ) ;
#1116 = DIRECTION ( 'NONE',  ( -0.6866640666150805039, 0.01727741078588136345, 0.7267695306602887095 ) ) ;
#1117 = ORIENTED_EDGE ( 'NONE', *, *, #2214, .T. ) ;
#1118 = CARTESIAN_POINT ( 'NONE',  ( 2.000000000000000000, 1.917977788252103204E-15, -15.66147716702868209 ) ) ;
#1119 = AXIS2_PLACEMENT_3D ( 'NONE', #4301, #646, #2135 ) ;
#1120 = CARTESIAN_POINT ( 'NONE',  ( 27.00000000000000355, 29.99999999999997158, 0.000000000000000000 ) ) ;
#1121 = EDGE_CURVE ( 'NONE', #2334, #6860, #2166, .T. ) ;
#1122 = CARTESIAN_POINT ( 'NONE',  ( -17.50000000000000355, 2.143131898507868643E-15, 0.000000000000000000 ) ) ;
#1123 = EDGE_CURVE ( 'NONE', #754, #5200, #1208, .T. ) ;
#1124 = CARTESIAN_POINT ( 'NONE',  ( 0.000000000000000000, 14.14213562373247868, 12.58213562373372341 ) ) ;
#1125 = EDGE_CURVE ( 'NONE', #3327, #6611, #5517, .T. ) ;
#1126 = EDGE_CURVE ( 'NONE', #1041, #1656, #729, .T. ) ;
#1127 = VECTOR ( 'NONE', #3429, 1000.000000000000000 ) ;
#1128 = LINE ( 'NONE', #9193, #1741 ) ;
#1129 = ORIENTED_EDGE ( 'NONE', *, *, #6545, .T. ) ;
#1130 = ORIENTED_EDGE ( 'NONE', *, *, #3044, .T. ) ;
#1131 = DIRECTION ( 'NONE',  ( -0.7071067811865445751, 0.5000000000000019984, 0.5000000000000024425 ) ) ;
#1132 = VERTEX_POINT ( 'NONE', #14 ) ;
#1133 = CARTESIAN_POINT ( 'NONE',  ( 0.000000000000000000, -22.50000000000000355, 5.000000000000000000 ) ) ;
#1134 = AXIS2_PLACEMENT_3D ( 'NONE', #6917, #5385, #7630 ) ;
#1135 = CARTESIAN_POINT ( 'NONE',  ( 26.65000000000001634, -4.333301281932499194, 0.000000000000000000 ) ) ;
#1136 = EDGE_LOOP ( 'NONE', ( #4865, #8916, #3783, #8298 ) ) ;
#1137 = FACE_OUTER_BOUND ( 'NONE', #1043, .T. ) ;
#1138 = DIRECTION ( 'NONE',  ( 0.7071067811865439090, 8.659560562354979697E-17, 0.7071067811865512365 ) ) ;
#1139 = ADVANCED_FACE ( 'NONE', ( #2318 ), #8173, .F. ) ;
#1140 = ADVANCED_FACE ( 'NONE', ( #7398 ), #5247, .F. ) ;
#1141 = CARTESIAN_POINT ( 'NONE',  ( 4.000000000000000000, -14.14213562373112154, 15.70213562373564820 ) ) ;
#1142 = CARTESIAN_POINT ( 'NONE',  ( -4.506465992502256768, -27.73646215562212092, 1.098439957185652682 ) ) ;
#1143 = ADVANCED_FACE ( 'NONE', ( #815 ), #2367, .F. ) ;
#1144 = ORIENTED_EDGE ( 'NONE', *, *, #4830, .F. ) ;
#1145 = ORIENTED_EDGE ( 'NONE', *, *, #7525, .T. ) ;
#1146 = LINE ( 'NONE', #6972, #1344 ) ;
#1147 = CARTESIAN_POINT ( 'NONE',  ( 38.00000000000000000, -43.00000000000000000, 11.99999999999999645 ) ) ;
#1148 = CARTESIAN_POINT ( 'NONE',  ( 0.000000000000000000, 22.50000000000000355, 2.000000000000013767 ) ) ;
#1149 = CARTESIAN_POINT ( 'NONE',  ( 0.000000000000000000, 0.000000000000000000, -22.00000000000000711 ) ) ;
#1150 = DIRECTION ( 'NONE',  ( 0.000000000000000000, 0.000000000000000000, 1.000000000000000000 ) ) ;
#1151 = AXIS2_PLACEMENT_3D ( 'NONE', #1715, #6193, #5467 ) ;
#1152 = CARTESIAN_POINT ( 'NONE',  ( 22.50000000000000355, 0.000000000000000000, 5.000000000000000000 ) ) ;
#1153 = EDGE_LOOP ( 'NONE', ( #3979, #2206 ) ) ;
#1154 = EDGE_LOOP ( 'NONE', ( #4904, #2784, #3254, #4832, #3865, #3227 ) ) ;
#1155 = CARTESIAN_POINT ( 'NONE',  ( -15.00000000000000000, 0.000000000000000000, 10.00000000000000000 ) ) ;
#1156 = DIRECTION ( 'NONE',  ( -0.000000000000000000, -0.000000000000000000, -1.000000000000000000 ) ) ;
#1157 = AXIS2_PLACEMENT_3D ( 'NONE', #2311, #6060, #1685 ) ;
#1158 = DIRECTION ( 'NONE',  ( -0.5773502691896251759, 0.5773502691896228445, -0.5773502691896293948 ) ) ;
#1159 = CARTESIAN_POINT ( 'NONE',  ( 0.000000000000000000, -22.50000000000000355, 0.000000000000000000 ) ) ;
#1160 = FACE_BOUND ( 'NONE', #7575, .T. ) ;
#1161 = VERTEX_POINT ( 'NONE', #3034 ) ;
#1162 = VECTOR ( 'NONE', #8268, 1000.000000000000000 ) ;
#1163 = VERTEX_POINT ( 'NONE', #7258 ) ;
#1164 = ORIENTED_EDGE ( 'NONE', *, *, #8986, .F. ) ;
#1165 = FACE_BOUND ( 'NONE', #7878, .T. ) ;
#1166 = CARTESIAN_POINT ( 'NONE',  ( 0.000000000000000000, 0.000000000000000000, 0.000000000000000000 ) ) ;
#1167 = DIRECTION ( 'NONE',  ( 0.000000000000000000, 0.7071067811865455743, -0.7071067811865494601 ) ) ;
#1168 = CONICAL_SURFACE ( 'NONE', #7456, 30.00000000000000000, 0.7853981633974488341 ) ;
#1169 = VECTOR ( 'NONE', #7368, 1000.000000000000000 ) ;
#1170 = DIRECTION ( 'NONE',  ( 0.000000000000000000, 0.000000000000000000, -1.000000000000000000 ) ) ;
#1171 =( REPRESENTATION_RELATIONSHIP ('NONE','NONE', #1933, #8501 ) REPRESENTATION_RELATIONSHIP_WITH_TRANSFORMATION ( #7195 )SHAPE_REPRESENTATION_RELATIONSHIP( ) );
#1172 = CARTESIAN_POINT ( 'NONE',  ( -22.50000000000000355, 0.000000000000000000, 2.000000000000039080 ) ) ;
#1173 = ORIENTED_EDGE ( 'NONE', *, *, #4774, .T. ) ;
#1174 = ORIENTED_EDGE ( 'NONE', *, *, #7702, .T. ) ;
#1175 = DIRECTION ( 'NONE',  ( 1.000000000000000000, 0.000000000000000000, 0.000000000000000000 ) ) ;
#1176 = ORIENTED_EDGE ( 'NONE', *, *, #3653, .T. ) ;
#1177 = AXIS2_PLACEMENT_3D ( 'NONE', #1549, #7407, #4527 ) ;
#1178 = EDGE_CURVE ( 'NONE', #8069, #1024, #6744, .T. ) ;
#1179 = DIRECTION ( 'NONE',  ( -1.000000000000000000, 0.000000000000000000, 0.000000000000000000 ) ) ;
#1180 = DIRECTION ( 'NONE',  ( -1.000000000000000000, 0.000000000000000000, 0.000000000000000000 ) ) ;
#1181 = ADVANCED_FACE ( 'NONE', ( #8793 ), #2213, .F. ) ;
#1182 = ORIENTED_EDGE ( 'NONE', *, *, #427, .T. ) ;
#1183 = CARTESIAN_POINT ( 'NONE',  ( -31.99999999999999289, 29.99999999999997868, 58.99999999999997158 ) ) ;
#1184 = FACE_OUTER_BOUND ( 'NONE', #3778, .T. ) ;
#1185 = AXIS2_PLACEMENT_3D ( 'NONE', #4041, #384, #7548 ) ;
#1186 = VECTOR ( 'NONE', #1880, 1000.000000000000000 ) ;
#1187 = AXIS2_PLACEMENT_3D ( 'NONE', #9074, #8215, #4762 ) ;
#1188 = DIRECTION ( 'NONE',  ( -0.000000000000000000, -0.000000000000000000, -1.000000000000000000 ) ) ;
#1189 = CARTESIAN_POINT ( 'NONE',  ( 27.45147183906050969, 5.102343880922168395, 0.9152318965389144578 ) ) ;
#1190 = EDGE_CURVE ( 'NONE', #5539, #5419, #4669, .T. ) ;
#1191 = VECTOR ( 'NONE', #191, 1000.000000000000000 ) ;
#1192 = ORIENTED_EDGE ( 'NONE', *, *, #6007, .F. ) ;
#1193 = ORIENTED_EDGE ( 'NONE', *, *, #4803, .T. ) ;
#1194 = APPLICATION_PROTOCOL_DEFINITION ( 'draft international standard', 'automotive_design', 1998, #8359 ) ;
#1195 =( GEOMETRIC_REPRESENTATION_CONTEXT ( 3 ) GLOBAL_UNCERTAINTY_ASSIGNED_CONTEXT ( ( #3839 ) ) GLOBAL_UNIT_ASSIGNED_CONTEXT ( ( #5393, #3130, #5485 ) ) REPRESENTATION_CONTEXT ( 'NONE', 'WORKASPACE' ) );
#1196 = DIRECTION ( 'NONE',  ( -1.000000000000000000, 0.000000000000000000, 0.000000000000000000 ) ) ;
#1197 = LINE ( 'NONE', #4988, #6656 ) ;
#1198 = CARTESIAN_POINT ( 'NONE',  ( -52.86930915046633572, 28.38475884032111196, -81.18159060786257442 ) ) ;
#1199 = ORIENTED_EDGE ( 'NONE', *, *, #8949, .T. ) ;
#1200 = EDGE_LOOP ( 'NONE', ( #3293, #365 ) ) ;
#1201 = AXIS2_PLACEMENT_3D ( 'NONE', #5797, #2183, #34 ) ;
#1202 = EDGE_LOOP ( 'NONE', ( #1388, #7892 ) ) ;
#1203 = AXIS2_PLACEMENT_3D ( 'NONE', #351, #1158, #6796 ) ;
#1204 = DIRECTION ( 'NONE',  ( 0.000000000000000000, 0.000000000000000000, 1.000000000000000000 ) ) ;
#1205 = FACE_OUTER_BOUND ( 'NONE', #3087, .T. ) ;
#1206 = DIRECTION ( 'NONE',  ( 0.000000000000000000, 0.000000000000000000, 1.000000000000000000 ) ) ;
#1207 = DIRECTION ( 'NONE',  ( 0.000000000000000000, 0.000000000000000000, 1.000000000000000000 ) ) ;
#1208 = CIRCLE ( 'NONE', #1360, 2.999999999999999112 ) ;
#1209 = CARTESIAN_POINT ( 'NONE',  ( 2.265596578422601819E-15, -34.99999999999999289, 50.49999999999998579 ) ) ;
#1210 = ORIENTED_EDGE ( 'NONE', *, *, #2888, .F. ) ;
#1211 = VERTEX_POINT ( 'NONE', #4574 ) ;
#1212 =( NAMED_UNIT ( * ) SI_UNIT ( $, .STERADIAN. ) SOLID_ANGLE_UNIT ( ) );
#1213 = ORIENTED_EDGE ( 'NONE', *, *, #6366, .F. ) ;
#1214 = DIRECTION ( 'NONE',  ( 1.000000000000000000, 0.000000000000000000, 0.000000000000000000 ) ) ;
#1215 = LINE ( 'NONE', #1358, #562 ) ;
#1216 = EDGE_CURVE ( 'NONE', #5087, #1485, #7499, .T. ) ;
#1217 = CARTESIAN_POINT ( 'NONE',  ( 28.44339478698105594, 0.8493939025105605722, 1.455282208020844514 ) ) ;
#1218 = EDGE_CURVE ( 'NONE', #9088, #8254, #2902, .T. ) ;
#1219 = CARTESIAN_POINT ( 'NONE',  ( -15.99999999999999645, -43.00000000000000000, 11.99999999999999645 ) ) ;
#1220 = EDGE_LOOP ( 'NONE', ( #628, #4675, #1579 ) ) ;
#1221 = EDGE_LOOP ( 'NONE', ( #2803, #124, #783, #1287 ) ) ;
#1222 = DIRECTION ( 'NONE',  ( 0.000000000000000000, 0.000000000000000000, 1.000000000000000000 ) ) ;
#1223 = ORIENTED_EDGE ( 'NONE', *, *, #2885, .F. ) ;
#1224 = CARTESIAN_POINT ( 'NONE',  ( 16.00000000000000000, -43.00000000000000000, -7.366666666666667140 ) ) ;
#1225 = CARTESIAN_POINT ( 'NONE',  ( -6.000000000000000888, -22.50000000000000355, 5.000000000000000000 ) ) ;
#1226 = CARTESIAN_POINT ( 'NONE',  ( 4.000000000000000000, 0.000000000000000000, 0.000000000000000000 ) ) ;
#1227 = FACE_OUTER_BOUND ( 'NONE', #292, .T. ) ;
#1228 = CARTESIAN_POINT ( 'NONE',  ( 4.000000000000000000, 7.653668647302530381, 18.47759065022802716 ) ) ;
#1229 = VECTOR ( 'NONE', #7520, 1000.000000000000000 ) ;
#1230 = CARTESIAN_POINT ( 'NONE',  ( 28.40723282374007042, 2.660173739710351981, 1.529649672404342242 ) ) ;
#1231 = ORIENTED_EDGE ( 'NONE', *, *, #2888, .T. ) ;
#1232 = ORIENTED_EDGE ( 'NONE', *, *, #1031, .F. ) ;
#1233 = PRODUCT_RELATED_PRODUCT_CATEGORY ( 'part', '', ( #2705 ) ) ;
#1234 = PRODUCT_DEFINITION_SHAPE ( 'NONE', 'NONE',  #9488 ) ;
#1235 = ADVANCED_FACE ( 'NONE', ( #299 ), #3268, .F. ) ;
#1236 = EDGE_CURVE ( 'NONE', #7815, #2124, #3224, .T. ) ;
#1237 = ADVANCED_FACE ( 'NONE', ( #7593 ), #8272, .T. ) ;
#1238 = DIRECTION ( 'NONE',  ( 8.659560562354994488E-17, 0.7071067811865426878, -0.7071067811865524577 ) ) ;
#1239 = FACE_OUTER_BOUND ( 'NONE', #6000, .T. ) ;
#1240 = EDGE_CURVE ( 'NONE', #4833, #3516, #249, .T. ) ;
#1241 = CARTESIAN_POINT ( 'NONE',  ( 0.000000000000000000, 0.000000000000000000, 20.00000000000000000 ) ) ;
#1242 = ORIENTED_EDGE ( 'NONE', *, *, #3296, .F. ) ;
#1243 = ORIENTED_EDGE ( 'NONE', *, *, #4505, .T. ) ;
#1244 = ORIENTED_EDGE ( 'NONE', *, *, #5697, .F. ) ;
#1245 = ORIENTED_EDGE ( 'NONE', *, *, #4252, .T. ) ;
#1246 = CARTESIAN_POINT ( 'NONE',  ( -25.50000000000000355, 0.000000000000000000, 10.00000000000000000 ) ) ;
#1247 = VECTOR ( 'NONE', #4632, 1000.000000000000000 ) ;
#1248 = LINE ( 'NONE', #3457, #2096 ) ;
#1249 = CARTESIAN_POINT ( 'NONE',  ( 4.000000000000000000, -18.47759065022790637, -6.903668647298391470 ) ) ;
#1250 = ADVANCED_FACE ( 'NONE', ( #3131 ), #906, .T. ) ;
#1251 = DIRECTION ( 'NONE',  ( -1.000000000000000000, 0.000000000000000000, 0.000000000000000000 ) ) ;
#1252 = FACE_BOUND ( 'NONE', #5996, .T. ) ;
#1253 = ADVANCED_FACE ( 'NONE', ( #918 ), #7189, .F. ) ;
#1254 = ORIENTED_EDGE ( 'NONE', *, *, #9320, .F. ) ;
#1255 = ORIENTED_EDGE ( 'NONE', *, *, #306, .T. ) ;
#1256 = CARTESIAN_POINT ( 'NONE',  ( 70.51394605043111596, 80.45324141007795049, 43.95616229837705191 ) ) ;
#1257 = EDGE_LOOP ( 'NONE', ( #1047, #1658, #1794, #3252 ) ) ;
#1258 = DIRECTION ( 'NONE',  ( 0.000000000000000000, 0.000000000000000000, -1.000000000000000000 ) ) ;
#1259 = CARTESIAN_POINT ( 'NONE',  ( -28.13653351783515788, 2.066994717595188824, 1.211640400093613179 ) ) ;
#1260 = FACE_OUTER_BOUND ( 'NONE', #5174, .T. ) ;
#1261 = DIRECTION ( 'NONE',  ( -1.000000000000000000, -0.000000000000000000, -0.000000000000000000 ) ) ;
#1262 = CARTESIAN_POINT ( 'NONE',  ( 5.000000000000000000, -14.14213562373248401, -14.14213562372942157 ) ) ;
#1263 = EDGE_LOOP ( 'NONE', ( #1622, #2699, #2434, #819, #7270, #3505 ) ) ;
#1264 = ORIENTED_EDGE ( 'NONE', *, *, #349, .T. ) ;
#1265 = LINE ( 'NONE', #5751, #7011 ) ;
#1266 = VERTEX_POINT ( 'NONE', #6885 ) ;
#1267 = CARTESIAN_POINT ( 'NONE',  ( -16.50000000000000000, 7.347880794884122694E-16, 2.000000000000039080 ) ) ;
#1268 = DIRECTION ( 'NONE',  ( 0.000000000000000000, 0.000000000000000000, 1.000000000000000000 ) ) ;
#1269 = CYLINDRICAL_SURFACE ( 'NONE', #1321, 7.250000000000002665 ) ;
#1270 = FACE_OUTER_BOUND ( 'NONE', #7923, .T. ) ;
#1271 = VECTOR ( 'NONE', #868, 1000.000000000000000 ) ;
#1272 = DIRECTION ( 'NONE',  ( -0.000000000000000000, -0.000000000000000000, 1.000000000000000000 ) ) ;
#1273 = ADVANCED_FACE ( 'NONE', ( #8981 ), #1734, .T. ) ;
#1274 = CARTESIAN_POINT ( 'NONE',  ( 26.42790562391195053, 6.696979066941341152, 0.2572250439434040636 ) ) ;
#1275 = ORIENTED_EDGE ( 'NONE', *, *, #6263, .T. ) ;
#1276 = ORIENTED_EDGE ( 'NONE', *, *, #3071, .F. ) ;
#1277 = CARTESIAN_POINT ( 'NONE',  ( 19.74999999999999645, -43.00000000000000000, -25.00000000000000000 ) ) ;
#1278 = CONTEXT_DEPENDENT_SHAPE_REPRESENTATION ( #3445, #6016 ) ;
#1279 = DIRECTION ( 'NONE',  ( 0.000000000000000000, 0.000000000000000000, 1.000000000000000000 ) ) ;
#1280 = CIRCLE ( 'NONE', #1134, 6.000000000000000888 ) ;
#1281 = DIRECTION ( 'NONE',  ( -0.000000000000000000, -0.000000000000000000, -1.000000000000000000 ) ) ;
#1282 = CIRCLE ( 'NONE', #3145, 3.000000000000002665 ) ;
#1283 = CARTESIAN_POINT ( 'NONE',  ( 53.29490495164537833, 15.90990257669733943, -88.90990257669730568 ) ) ;
#1284 = CARTESIAN_POINT ( 'NONE',  ( 15.00000000000000000, 1.836970198721029589E-15, 20.00000000000000000 ) ) ;
#1285 = ORIENTED_EDGE ( 'NONE', *, *, #4216, .F. ) ;
#1286 = VERTEX_POINT ( 'NONE', #6928 ) ;
#1287 = ORIENTED_EDGE ( 'NONE', *, *, #1925, .F. ) ;
#1288 = EDGE_CURVE ( 'NONE', #8082, #2348, #2509, .T. ) ;
#1289 = EDGE_LOOP ( 'NONE', ( #3491, #8589 ) ) ;
#1290 = ADVANCED_FACE ( 'NONE', ( #3944 ), #5350, .F. ) ;
#1291 = CARTESIAN_POINT ( 'NONE',  ( 5.000000000000000000, 9.605605015555367541E-13, 18.44000000000276884 ) ) ;
#1292 = AXIS2_PLACEMENT_3D ( 'NONE', #476, #7099, #7062 ) ;
#1293 = EDGE_CURVE ( 'NONE', #7976, #5380, #6870, .T. ) ;
#1294 = EDGE_CURVE ( 'NONE', #9088, #1890, #5486, .T. ) ;
#1295 = APPLICATION_CONTEXT ( 'automotive_design' ) ;
#1296 = DIRECTION ( 'NONE',  ( -0.000000000000000000, -0.000000000000000000, -1.000000000000000000 ) ) ;
#1297 = AXIS2_PLACEMENT_3D ( 'NONE', #3610, #8890, #1641 ) ;
#1298 = DIRECTION ( 'NONE',  ( 0.000000000000000000, 0.000000000000000000, -1.000000000000000000 ) ) ;
#1299 = CYLINDRICAL_SURFACE ( 'NONE', #4634, 2.999999999999999112 ) ;
#1300 = DIRECTION ( 'NONE',  ( 1.000000000000000000, 0.000000000000000000, 0.000000000000000000 ) ) ;
#1301 = ORIENTED_EDGE ( 'NONE', *, *, #7281, .T. ) ;
#1302 = CARTESIAN_POINT ( 'NONE',  ( -60.00000000000000000, 0.000000000000000000, -30.00000000000000000 ) ) ;
#1303 = ORIENTED_EDGE ( 'NONE', *, *, #830, .F. ) ;
#1304 = DIRECTION ( 'NONE',  ( 0.000000000000000000, 0.000000000000000000, -1.000000000000000000 ) ) ;
#1305 = FACE_BOUND ( 'NONE', #6622, .T. ) ;
#1306 = CARTESIAN_POINT ( 'NONE',  ( -26.64999999999998792, 4.333301281932682159, 0.000000000000000000 ) ) ;
#1307 =( BOUNDED_CURVE ( )  B_SPLINE_CURVE ( 3, ( #333, #1628, #3887, #4756 ),
 .UNSPECIFIED., .F., .T. ) 
 B_SPLINE_CURVE_WITH_KNOTS ( ( 4, 4 ),
 ( 0.000000000000000000, 0.7853981633974483900 ),
 .UNSPECIFIED. ) 
 CURVE ( )  GEOMETRIC_REPRESENTATION_ITEM ( )  RATIONAL_B_SPLINE_CURVE ( ( 1.000000000000000000, 0.9492530216741911220, 0.9492530216741911220, 1.000000000000000000 ) ) 
 REPRESENTATION_ITEM ( '' )  );
#1308 = ADVANCED_FACE ( 'NONE', ( #4620 ), #1102, .F. ) ;
#1309 = DIRECTION ( 'NONE',  ( 0.000000000000000000, 0.000000000000000000, 1.000000000000000000 ) ) ;
#1310 = DIRECTION ( 'NONE',  ( -1.000000000000000000, -0.000000000000000000, -0.000000000000000000 ) ) ;
#1311 = VECTOR ( 'NONE', #5911, 1000.000000000000000 ) ;
#1312 = DIRECTION ( 'NONE',  ( -0.7071067811865435759, 0.000000000000000000, 0.7071067811865514585 ) ) ;
#1313 = ORIENTED_EDGE ( 'NONE', *, *, #4357, .F. ) ;
#1314 = ADVANCED_FACE ( 'NONE', ( #965 ), #9034, .F. ) ;
#1315 = ORIENTED_EDGE ( 'NONE', *, *, #728, .F. ) ;
#1316 = CARTESIAN_POINT ( 'NONE',  ( 37.00000000000000000, -15.90990257669733943, -54.09009742330271564 ) ) ;
#1317 = ORIENTED_EDGE ( 'NONE', *, *, #2600, .F. ) ;
#1318 = DIRECTION ( 'NONE',  ( -1.000000000000000000, 0.000000000000000000, 0.000000000000000000 ) ) ;
#1319 = DIRECTION ( 'NONE',  ( -1.000000000000000000, 1.224646799147353454E-16, 0.000000000000000000 ) ) ;
#1320 = CARTESIAN_POINT ( 'NONE',  ( -28.00000000000000711, 0.000000000000000000, 10.00000000000000000 ) ) ;
#1321 = AXIS2_PLACEMENT_3D ( 'NONE', #8626, #5799, #9393 ) ;
#1322 =( GEOMETRIC_REPRESENTATION_CONTEXT ( 3 ) GLOBAL_UNCERTAINTY_ASSIGNED_CONTEXT ( ( #3073 ) ) GLOBAL_UNIT_ASSIGNED_CONTEXT ( ( #6901, #7607, #6034 ) ) REPRESENTATION_CONTEXT ( 'NONE', 'WORKASPACE' ) );
#1323 = CARTESIAN_POINT ( 'NONE',  ( -38.00000000000000711, 43.00000000000000000, -7.366666666666667140 ) ) ;
#1324 = CARTESIAN_POINT ( 'NONE',  ( -27.00000000000000000, 43.00000000000000000, 11.99999999999999645 ) ) ;
#1325 = CLOSED_SHELL ( 'NONE', ( #9219, #1250, #511, #3300, #532, #4442, #396, #7245, #8155, #1469, #4846, #3506, #619, #3243, #5676, #7534, #7289, #8858, #1454, #2663, #4713, #5237, #8409, #1273, #4731, #7646, #599, #5301, #5182, #2175 ) ) ;
#1326 = CARTESIAN_POINT ( 'NONE',  ( -38.00000000000000711, 43.00000000000000000, -7.366666666666667140 ) ) ;
#1327 = CIRCLE ( 'NONE', #6708, 3.000000000000002665 ) ;
#1328 = ORIENTED_EDGE ( 'NONE', *, *, #9361, .T. ) ;
#1329 = ORIENTED_EDGE ( 'NONE', *, *, #8935, .F. ) ;
#1330 =( GEOMETRIC_REPRESENTATION_CONTEXT ( 3 ) GLOBAL_UNCERTAINTY_ASSIGNED_CONTEXT ( ( #7388 ) ) GLOBAL_UNIT_ASSIGNED_CONTEXT ( ( #7074, #8516, #1935 ) ) REPRESENTATION_CONTEXT ( 'NONE', 'WORKASPACE' ) );
#1331 = CARTESIAN_POINT ( 'NONE',  ( -51.96152422706632734, 30.00000000000000000, -134.0000000000000284 ) ) ;
#1332 = VECTOR ( 'NONE', #4765, 1000.000000000000000 ) ;
#1333 = AXIS2_PLACEMENT_3D ( 'NONE', #7194, #7239, #1380 ) ;
#1334 = DIRECTION ( 'NONE',  ( -1.000000000000000000, 0.000000000000000000, 0.000000000000000000 ) ) ;
#1335 = EDGE_CURVE ( 'NONE', #4792, #3327, #7628, .T. ) ;
#1336 = AXIS2_PLACEMENT_3D ( 'NONE', #239, #3014, #3162 ) ;
#1337 = DIRECTION ( 'NONE',  ( 0.000000000000000000, 0.000000000000000000, 1.000000000000000000 ) ) ;
#1338 = CARTESIAN_POINT ( 'NONE',  ( -28.50000000000000355, 0.000000000000000000, 5.000000000000000000 ) ) ;
#1339 = AXIS2_PLACEMENT_3D ( 'NONE', #2961, #2869, #5850 ) ;
#1340 = ORIENTED_EDGE ( 'NONE', *, *, #9033, .F. ) ;
#1341 = EDGE_CURVE ( 'NONE', #5088, #1397, #4987, .T. ) ;
#1342 = ORIENTED_EDGE ( 'NONE', *, *, #3024, .T. ) ;
#1343 = ORIENTED_EDGE ( 'NONE', *, *, #6945, .F. ) ;
#1344 = VECTOR ( 'NONE', #7015, 1000.000000000000114 ) ;
#1345 = ORIENTED_EDGE ( 'NONE', *, *, #153, .F. ) ;
#1346 = CARTESIAN_POINT ( 'NONE',  ( 28.26575725008336093, -1.673027373761835079, 1.314514334795901185 ) ) ;
#1347 = DIRECTION ( 'NONE',  ( -0.000000000000000000, -0.000000000000000000, -1.000000000000000000 ) ) ;
#1348 = DIRECTION ( 'NONE',  ( 1.000000000000000000, 0.000000000000000000, 0.000000000000000000 ) ) ;
#1349 = CARTESIAN_POINT ( 'NONE',  ( 22.50000000000000355, 2.356749903719115078E-13, 15.00000000000000000 ) ) ;
#1350 = DIRECTION ( 'NONE',  ( -1.000000000000000000, 0.000000000000000000, 0.000000000000000000 ) ) ;
#1351 = CIRCLE ( 'NONE', #6739, 28.00000000000000711 ) ;
#1352 = VECTOR ( 'NONE', #9344, 1000.000000000000114 ) ;
#1353 = ORIENTED_EDGE ( 'NONE', *, *, #8809, .T. ) ;
#1354 = AXIS2_PLACEMENT_3D ( 'NONE', #2476, #5401, #6176 ) ;
#1355 = DIRECTION ( 'NONE',  ( 0.000000000000000000, 0.000000000000000000, -1.000000000000000000 ) ) ;
#1356 = ORIENTED_EDGE ( 'NONE', *, *, #4938, .F. ) ;
#1357 = DIRECTION ( 'NONE',  ( 0.000000000000000000, 0.000000000000000000, 1.000000000000000000 ) ) ;
#1358 = CARTESIAN_POINT ( 'NONE',  ( -3.000000000000000444, 0.000000000000000000, 21.00000000000000000 ) ) ;
#1359 = EDGE_CURVE ( 'NONE', #2727, #6154, #4177, .T. ) ;
#1360 = AXIS2_PLACEMENT_3D ( 'NONE', #8939, #7304, #9469 ) ;
#1362 = EDGE_CURVE ( 'NONE', #334, #9368, #7161, .T. ) ;
#1361 = CARTESIAN_POINT ( 'NONE',  ( 37.22467645238199196, 47.05659850664387278, -5.608807313787652404 ) ) ;
#1363 = LINE ( 'NONE', #1455, #9425 ) ;
#1364 = CARTESIAN_POINT ( 'NONE',  ( -4.333301281932591564, -26.65000000000000213, 0.000000000000000000 ) ) ;
#1365 = ORIENTED_EDGE ( 'NONE', *, *, #8414, .F. ) ;
#1366 = ORIENTED_EDGE ( 'NONE', *, *, #2068, .T. ) ;
#1367 = CARTESIAN_POINT ( 'NONE',  ( 0.7500000000000000000, 0.7500000000000000000, 0.000000000000000000 ) ) ;
#1368 = VERTEX_POINT ( 'NONE', #9259 ) ;
#1369 = CARTESIAN_POINT ( 'NONE',  ( 27.00000000000000000, -43.00000000000000000, 11.99999999999999645 ) ) ;
#1370 = DIRECTION ( 'NONE',  ( 0.7071067811865493491, -1.126022036214515194E-15, -0.7071067811865455743 ) ) ;
#1371 =( BOUNDED_CURVE ( )  B_SPLINE_CURVE ( 3, ( #7360, #8712, #111, #2172 ),
 .UNSPECIFIED., .F., .T. ) 
 B_SPLINE_CURVE_WITH_KNOTS ( ( 4, 4 ),
 ( 2.356194490192345281, 3.926990816987240951 ),
 .UNSPECIFIED. ) 
 CURVE ( )  GEOMETRIC_REPRESENTATION_ITEM ( )  RATIONAL_B_SPLINE_CURVE ( ( 1.000000000000000000, 0.8047378541243652705, 0.8047378541243652705, 1.000000000000000000 ) ) 
 REPRESENTATION_ITEM ( '' )  );
#1372 = CARTESIAN_POINT ( 'NONE',  ( 60.00000000000000000, -15.90990257669733943, -85.90990257669729147 ) ) ;
#1373 = EDGE_CURVE ( 'NONE', #4405, #2727, #5170, .T. ) ;
#1374 = FACE_OUTER_BOUND ( 'NONE', #2741, .T. ) ;
#1375 = CIRCLE ( 'NONE', #5968, 60.00000000000000000 ) ;
#1376 = DIRECTION ( 'NONE',  ( 1.000000000000000000, -0.000000000000000000, -0.000000000000000000 ) ) ;
#1377 = DIRECTION ( 'NONE',  ( -1.000000000000000000, 0.000000000000000000, 0.000000000000000000 ) ) ;
#1378 = ORIENTED_EDGE ( 'NONE', *, *, #5924, .F. ) ;
#1379 = ORIENTED_EDGE ( 'NONE', *, *, #4011, .T. ) ;
#1380 = DIRECTION ( 'NONE',  ( 0.000000000000000000, 0.000000000000000000, 1.000000000000000000 ) ) ;
#1381 = CONTEXT_DEPENDENT_SHAPE_REPRESENTATION ( #6103, #8763 ) ;
#1382 = LINE ( 'NONE', #3494, #1802 ) ;
#1383 = AXIS2_PLACEMENT_3D ( 'NONE', #8049, #8244, #2231 ) ;
#1384 = CARTESIAN_POINT ( 'NONE',  ( 3.000000000000000000, 22.50000000000000355, 10.00000000000000000 ) ) ;
#1385 = DIRECTION ( 'NONE',  ( 0.000000000000000000, 0.000000000000000000, 1.000000000000000000 ) ) ;
#1386 = EDGE_LOOP ( 'NONE', ( #9060, #4980, #3350 ) ) ;
#1387 = ORIENTED_EDGE ( 'NONE', *, *, #8390, .F. ) ;
#1388 = ORIENTED_EDGE ( 'NONE', *, *, #3626, .F. ) ;
#1389 = CIRCLE ( 'NONE', #3853, 15.00000000000000000 ) ;
#1390 = ORIENTED_EDGE ( 'NONE', *, *, #7995, .T. ) ;
#1391 = DIRECTION ( 'NONE',  ( 1.000000000000000000, -0.000000000000000000, -0.000000000000000000 ) ) ;
#1392 = DIRECTION ( 'NONE',  ( -1.000000000000000000, 0.000000000000000000, 0.000000000000000000 ) ) ;
#1393 = EDGE_CURVE ( 'NONE', #5764, #2437, #574, .T. ) ;
#1394 = DIRECTION ( 'NONE',  ( 0.000000000000000000, 0.000000000000000000, 1.000000000000000000 ) ) ;
#1395 = CARTESIAN_POINT ( 'NONE',  ( -27.74194578790376653, -4.529188556225802742, 1.101965149366714192 ) ) ;
#1396 = CYLINDRICAL_SURFACE ( 'NONE', #9154, 0.7499999999982936982 ) ;
#1397 = VERTEX_POINT ( 'NONE', #522 ) ;
#1398 = CARTESIAN_POINT ( 'NONE',  ( 37.00000000000000000, 30.00000000000000000, -13.00000000000001066 ) ) ;
#1399 = ORIENTED_EDGE ( 'NONE', *, *, #5814, .T. ) ;
#1400 = AXIS2_PLACEMENT_3D ( 'NONE', #5402, #4096, #9184 ) ;
#1401 = DIRECTION ( 'NONE',  ( -1.000000000000000000, 0.000000000000000000, 0.000000000000000000 ) ) ;
#1402 = EDGE_CURVE ( 'NONE', #6136, #8845, #5647, .T. ) ;
#1403 = PLANE ( 'NONE',  #5641 ) ;
#1404 = DIRECTION ( 'NONE',  ( 0.000000000000000000, 0.7071067811865479058, -0.7071067811865472397 ) ) ;
#1405 = CARTESIAN_POINT ( 'NONE',  ( 48.15955140082796504, 36.58521010404106732, -10.14640895491553252 ) ) ;
#1406 = AXIS2_PLACEMENT_3D ( 'NONE', #298, #9077, #3313 ) ;
#1407 = CARTESIAN_POINT ( 'NONE',  ( -0.4129292217235346896, -28.50085334706576035, 1.500673695285822395 ) ) ;
#1408 = ORIENTED_EDGE ( 'NONE', *, *, #4238, .F. ) ;
#1409 = ORIENTED_EDGE ( 'NONE', *, *, #7594, .T. ) ;
#1410 = AXIS2_PLACEMENT_3D ( 'NONE', #8798, #8847, #3041 ) ;
#1411 = ORIENTED_EDGE ( 'NONE', *, *, #3657, .F. ) ;
#1412 = DIRECTION ( 'NONE',  ( 0.6785983445458485530, -0.2810846377148105701, 0.6785983445458495522 ) ) ;
#1413 = EDGE_CURVE ( 'NONE', #5812, #6191, #2694, .T. ) ;
#1414 = CARTESIAN_POINT ( 'NONE',  ( 16.50000000000000000, 2.356749903719115078E-13, 5.000000000000000000 ) ) ;
#1415 = DIRECTION ( 'NONE',  ( 0.000000000000000000, 0.000000000000000000, 1.000000000000000000 ) ) ;
#1416 = ADVANCED_FACE ( 'NONE', ( #7064 ), #3449, .F. ) ;
#1417 = ADVANCED_FACE ( 'NONE', ( #3499 ), #6448, .T. ) ;
#1418 = EDGE_CURVE ( 'NONE', #7789, #3651, #3022, .T. ) ;
#1419 = CARTESIAN_POINT ( 'NONE',  ( 5.000000000000000000, -20.00000000000120437, 2.661998082081668380E-12 ) ) ;
#1420 = VECTOR ( 'NONE', #5369, 1000.000000000000114 ) ;
#1421 = DIRECTION ( 'NONE',  ( 0.000000000000000000, 0.000000000000000000, 1.000000000000000000 ) ) ;
#1422 = DIRECTION ( 'NONE',  ( -1.000000000000000000, -0.000000000000000000, -0.000000000000000000 ) ) ;
#1423 = ORIENTED_EDGE ( 'NONE', *, *, #4319, .T. ) ;
#1424 = ORIENTED_EDGE ( 'NONE', *, *, #7147, .T. ) ;
#1425 = CARTESIAN_POINT ( 'NONE',  ( -15.99999999999999645, -43.00000000000000000, -7.366666666666667140 ) ) ;
#1426 = EDGE_CURVE ( 'NONE', #4458, #95, #2789, .T. ) ;
#1427 = VECTOR ( 'NONE', #1736, 1000.000000000000000 ) ;
#1428 = EDGE_CURVE ( 'NONE', #3148, #7251, #5582, .T. ) ;
#1429 = DIRECTION ( 'NONE',  ( 0.7071067811865441310, -0.7071067811865507924, -0.000000000000000000 ) ) ;
#1430 = EDGE_CURVE ( 'NONE', #6915, #2915, #1491, .T. ) ;
#1431 = LINE ( 'NONE', #5084, #4054 ) ;
#1432 = DIRECTION ( 'NONE',  ( 1.000000000000000000, 0.000000000000000000, 0.000000000000000000 ) ) ;
#1433 = ORIENTED_EDGE ( 'NONE', *, *, #7153, .F. ) ;
#1434 = VERTEX_POINT ( 'NONE', #4087 ) ;
#1435 = VERTEX_POINT ( 'NONE', #3365 ) ;
#1436 = DIRECTION ( 'NONE',  ( 0.7269748686300442353, 0.01631937727526915766, 0.6864701146486112959 ) ) ;
#1437 = ORIENTED_EDGE ( 'NONE', *, *, #7525, .F. ) ;
#1438 = VECTOR ( 'NONE', #8497, 1000.000000000000000 ) ;
#1439 = CARTESIAN_POINT ( 'NONE',  ( 27.16490240584779059, -3.793344078502343564, 0.4263419363949833008 ) ) ;
#1440 = FACE_OUTER_BOUND ( 'NONE', #5060, .T. ) ;
#1441 = AXIS2_PLACEMENT_3D ( 'NONE', #7017, #9256, #2015 ) ;
#1442 = CARTESIAN_POINT ( 'NONE',  ( 0.000000000000000000, 22.50000000000000355, 0.000000000000000000 ) ) ;
#1443 = DIRECTION ( 'NONE',  ( -1.000000000000000000, 0.000000000000000000, 0.000000000000000000 ) ) ;
#1444 = CARTESIAN_POINT ( 'NONE',  ( 0.000000000000000000, 0.000000000000000000, 1.000000000000000000 ) ) ;
#1445 = AXIS2_PLACEMENT_3D ( 'NONE', #1467, #4496, #8107 ) ;
#1446 = FACE_BOUND ( 'NONE', #7222, .T. ) ;
#1447 = ORIENTED_EDGE ( 'NONE', *, *, #8984, .T. ) ;
#1448 = FACE_OUTER_BOUND ( 'NONE', #5684, .T. ) ;
#1449 = VECTOR ( 'NONE', #5531, 999.9999999999998863 ) ;
#1450 = ORIENTED_EDGE ( 'NONE', *, *, #6945, .T. ) ;
#1451 = CARTESIAN_POINT ( 'NONE',  ( 0.000000000000000000, 0.000000000000000000, 10.00000000000000000 ) ) ;
#1452 = DIRECTION ( 'NONE',  ( 0.000000000000000000, 0.000000000000000000, 1.000000000000000000 ) ) ;
#1453 = DIRECTION ( 'NONE',  ( -1.000000000000000000, 0.000000000000000000, 0.000000000000000000 ) ) ;
#1454 = ADVANCED_FACE ( 'NONE', ( #6308 ), #9213, .F. ) ;
#1455 = CARTESIAN_POINT ( 'NONE',  ( 60.00000000000000000, 12.50000000000000000, -100.0000000000000000 ) ) ;
#1456 = EDGE_LOOP ( 'NONE', ( #2022, #930 ) ) ;
#1457 = CIRCLE ( 'NONE', #3172, 8.000000000000021316 ) ;
#1458 = ORIENTED_EDGE ( 'NONE', *, *, #2101, .F. ) ;
#1459 = DIRECTION ( 'NONE',  ( 0.000000000000000000, 0.000000000000000000, 1.000000000000000000 ) ) ;
#1460 = ORIENTED_EDGE ( 'NONE', *, *, #8353, .T. ) ;
#1461 = DIRECTION ( 'NONE',  ( -1.000000000000000000, 0.000000000000000000, 0.000000000000000000 ) ) ;
#1462 = FACE_OUTER_BOUND ( 'NONE', #8040, .T. ) ;
#1463 = DIRECTION ( 'NONE',  ( 0.000000000000000000, 0.000000000000000000, -1.000000000000000000 ) ) ;
#1464 = DIRECTION ( 'NONE',  ( 1.000000000000000000, 0.000000000000000000, 0.000000000000000000 ) ) ;
#1465 = AXIS2_PLACEMENT_3D ( 'NONE', #9229, #1846, #8609 ) ;
#1466 = DIRECTION ( 'NONE',  ( 1.000000000000000000, 0.000000000000000000, -0.000000000000000000 ) ) ;
#1467 = CARTESIAN_POINT ( 'NONE',  ( -22.50000000000000000, -7.855833012397050680E-14, 5.000000000000000000 ) ) ;
#1468 = CARTESIAN_POINT ( 'NONE',  ( -53.29490495164537833, 15.90990257669733943, -85.90990257669729147 ) ) ;
#1469 = ADVANCED_FACE ( 'NONE', ( #7921 ), #7785, .T. ) ;
#1470 = ORIENTED_EDGE ( 'NONE', *, *, #8299, .T. ) ;
#1471 = VERTEX_POINT ( 'NONE', #4507 ) ;
#1472 = AXIS2_PLACEMENT_3D ( 'NONE', #1372, #2820, #4887 ) ;
#1473 = CARTESIAN_POINT ( 'NONE',  ( 27.00000000000000355, 35.00000000000000000, 64.00000000000000000 ) ) ;
#1474 = FACE_OUTER_BOUND ( 'NONE', #2115, .T. ) ;
#1475 = EDGE_CURVE ( 'NONE', #7481, #1766, #2921, .T. ) ;
#1476 = AXIS2_PLACEMENT_3D ( 'NONE', #9053, #6229, #358 ) ;
#1477 = DIRECTION ( 'NONE',  ( 1.000000000000000000, 0.000000000000000000, 0.000000000000000000 ) ) ;
#1478 = APPLICATION_CONTEXT ( 'automotive_design' ) ;
#1479 = CARTESIAN_POINT ( 'NONE',  ( -53.29490495164537833, -27.56180520566615044, -41.61356529332876875 ) ) ;
#1480 = ORIENTED_EDGE ( 'NONE', *, *, #1824, .F. ) ;
#1481 = EDGE_LOOP ( 'NONE', ( #3444, #9188, #552, #1232 ) ) ;
#1482 = ORIENTED_EDGE ( 'NONE', *, *, #1551, .T. ) ;
#1483 = AXIS2_PLACEMENT_3D ( 'NONE', #7199, #7831, #8644 ) ;
#1484 = DIRECTION ( 'NONE',  ( 1.734723475976807094E-18, 0.9997175446104180629, -0.02376617340079523882 ) ) ;
#1485 = VERTEX_POINT ( 'NONE', #2880 ) ;
#1486 = AXIS2_PLACEMENT_3D ( 'NONE', #8756, #6607, #5205 ) ;
#1487 = DIRECTION ( 'NONE',  ( 0.000000000000000000, 0.000000000000000000, -1.000000000000000000 ) ) ;
#1488 = DIRECTION ( 'NONE',  ( -0.000000000000000000, -0.000000000000000000, 1.000000000000000000 ) ) ;
#1489 = AXIS2_PLACEMENT_3D ( 'NONE', #7918, #2918, #5041 ) ;
#1490 = CARTESIAN_POINT ( 'NONE',  ( 53.29490495164537833, -3.673940397442057600E-15, -55.00000000000000711 ) ) ;
#1491 = CIRCLE ( 'NONE', #1483, 3.000000000000002665 ) ;
#1492 = CARTESIAN_POINT ( 'NONE',  ( 4.333301281932962823, -26.64999999999994529, 0.000000000000000000 ) ) ;
#1493 = VECTOR ( 'NONE', #6527, 1000.000000000000000 ) ;
#1494 = DIRECTION ( 'NONE',  ( 0.000000000000000000, 0.000000000000000000, -1.000000000000000000 ) ) ;
#1495 = AXIS2_PLACEMENT_3D ( 'NONE', #1929, #5636, #4094 ) ;
#1496 = CARTESIAN_POINT ( 'NONE',  ( 0.000000000000000000, 9.605605015555367541E-13, 18.44000000000276884 ) ) ;
#1497 = EDGE_LOOP ( 'NONE', ( #8449, #7236 ) ) ;
#1498 = DIRECTION ( 'NONE',  ( -1.000000000000000000, -0.000000000000000000, -0.000000000000000000 ) ) ;
#1499 = CIRCLE ( 'NONE', #3349, 6.000000000000001776 ) ;
#1500 = VERTEX_POINT ( 'NONE', #8165 ) ;
#1501 = CARTESIAN_POINT ( 'NONE',  ( -27.00000000000000000, 43.00000000000000000, 11.99999999999999645 ) ) ;
#1502 = CARTESIAN_POINT ( 'NONE',  ( 0.000000000000000000, -7.653668647303860872, -17.72759065022311731 ) ) ;
#1503 = CYLINDRICAL_SURFACE ( 'NONE', #7807, 6.000000000000000888 ) ;
#1504 = CIRCLE ( 'NONE', #7650, 6.000000000000001776 ) ;
#1505 = CARTESIAN_POINT ( 'NONE',  ( -9.048619709455117288, 15.70011763207404520, 47.70011763207404698 ) ) ;
#1506 = ORIENTED_EDGE ( 'NONE', *, *, #144, .T. ) ;
#1507 = ORIENTED_EDGE ( 'NONE', *, *, #5423, .F. ) ;
#1508 = LINE ( 'NONE', #649, #691 ) ;
#1509 = ORIENTED_EDGE ( 'NONE', *, *, #1123, .F. ) ;
#1510 = ADVANCED_FACE ( 'NONE', ( #5185 ), #2308, .T. ) ;
#1511 = CARTESIAN_POINT ( 'NONE',  ( 0.000000000000000000, -14.14213562373112154, 14.14213562373418220 ) ) ;
#1512 = LINE ( 'NONE', #35, #8565 ) ;
#1513 = AXIS2_PLACEMENT_3D ( 'NONE', #2817, #3389, #5754 ) ;
#1514 = DIRECTION ( 'NONE',  ( 0.000000000000000000, 0.000000000000000000, 1.000000000000000000 ) ) ;
#1515 = AXIS2_PLACEMENT_3D ( 'NONE', #6650, #3043, #3811 ) ;
#1516 = DIRECTION ( 'NONE',  ( 0.000000000000000000, 0.000000000000000000, 1.000000000000000000 ) ) ;
#1517 = EDGE_CURVE ( 'NONE', #5309, #75, #5918, .T. ) ;
#1518 = DIRECTION ( 'NONE',  ( 1.000000000000000000, 0.000000000000000000, 0.000000000000000000 ) ) ;
#1519 = CARTESIAN_POINT ( 'NONE',  ( -22.50000000000000355, 0.000000000000000000, 5.000000000000000000 ) ) ;
#1520 = CARTESIAN_POINT ( 'NONE',  ( 4.000000000000000000, 20.00000000000120437, 7.412591687719288072E-13 ) ) ;
#1521 = ORIENTED_EDGE ( 'NONE', *, *, #7864, .T. ) ;
#1522 = VERTEX_POINT ( 'NONE', #5233 ) ;
#1523 = CARTESIAN_POINT ( 'NONE',  ( -53.29490495164537833, -15.90990257669733943, -82.90990257669729147 ) ) ;
#1524 = ORIENTED_EDGE ( 'NONE', *, *, #2533, .F. ) ;
#1525 = EDGE_CURVE ( 'NONE', #1041, #6239, #3642, .T. ) ;
#1526 = LINE ( 'NONE', #7385, #5346 ) ;
#1527 = FACE_BOUND ( 'NONE', #8238, .T. ) ;
#1528 = UNCERTAINTY_MEASURE_WITH_UNIT (LENGTH_MEASURE( 1.000000000000000082E-05 ), #5211, 'distance_accuracy_value', 'NONE');
#1529 = DIRECTION ( 'NONE',  ( 0.000000000000000000, 0.000000000000000000, -1.000000000000000000 ) ) ;
#1530 = ORIENTED_EDGE ( 'NONE', *, *, #8852, .F. ) ;
#1531 = ORIENTED_EDGE ( 'NONE', *, *, #5481, .F. ) ;
#1532 = EDGE_CURVE ( 'NONE', #4339, #5838, #2201, .T. ) ;
#1533 = DIRECTION ( 'NONE',  ( 1.000000000000000000, -1.230442330444825458E-16, -1.005078904769186206E-16 ) ) ;
#1534 = VERTEX_POINT ( 'NONE', #5135 ) ;
#1535 = EDGE_CURVE ( 'NONE', #1500, #6154, #1028, .T. ) ;
#1536 = EDGE_CURVE ( 'NONE', #313, #1132, #7937, .T. ) ;
#1537 = CARTESIAN_POINT ( 'NONE',  ( -2.749999999999995559, 0.7500000000000000000, 1.500000000000000000 ) ) ;
#1538 = DIRECTION ( 'NONE',  ( -0.000000000000000000, -0.000000000000000000, -1.000000000000000000 ) ) ;
#1539 = ADVANCED_FACE ( 'NONE', ( #803 ), #1578, .F. ) ;
#1540 = CARTESIAN_POINT ( 'NONE',  ( -0.7500000000000000000, 2.750000000000002665, 1.500000000000000000 ) ) ;
#1541 = DIRECTION ( 'NONE',  ( -1.000000000000000000, 0.000000000000000000, 0.000000000000000000 ) ) ;
#1542 = CARTESIAN_POINT ( 'NONE',  ( 0.000000000000000000, 14.14213562373112154, -12.58213562373077821 ) ) ;
#1543 = CARTESIAN_POINT ( 'NONE',  ( 12.37436867076458036, 12.37436867076458036, 19.62563132923542142 ) ) ;
#1544 = CIRCLE ( 'NONE', #6922, 18.50000000000000355 ) ;
#1545 = EDGE_LOOP ( 'NONE', ( #4724, #465, #3693, #6289 ) ) ;
#1546 = DIRECTION ( 'NONE',  ( 0.000000000000000000, 0.000000000000000000, -1.000000000000000000 ) ) ;
#1547 = ORIENTED_EDGE ( 'NONE', *, *, #3751, .T. ) ;
#1548 = CARTESIAN_POINT ( 'NONE',  ( 16.00000000000000000, -43.00000000000000000, -7.366666666666667140 ) ) ;
#1549 = CARTESIAN_POINT ( 'NONE',  ( 0.000000000000000000, 22.50000000000000355, 5.000000000000000000 ) ) ;
#1550 = ADVANCED_FACE ( 'NONE', ( #6629 ), #9466, .T. ) ;
#1551 = EDGE_CURVE ( 'NONE', #3216, #6009, #2254, .T. ) ;
#1552 = CARTESIAN_POINT ( 'NONE',  ( -59.00000000000000000, 0.000000000000000000, 25.00000000000000000 ) ) ;
#1553 = CARTESIAN_POINT ( 'NONE',  ( -4.703319286132082944, 17.49999999999999645, 49.50000000000000000 ) ) ;
#1554 = EDGE_CURVE ( 'NONE', #2195, #4316, #3741, .T. ) ;
#1555 = EDGE_LOOP ( 'NONE', ( #5705, #6411, #9134, #661 ) ) ;
#1556 = AXIS2_PLACEMENT_3D ( 'NONE', #8802, #7509, #2223 ) ;
#1557 = PRODUCT_DEFINITION_SHAPE ( 'NONE', 'NONE',  #8051 ) ;
#1558 = ORIENTED_EDGE ( 'NONE', *, *, #841, .F. ) ;
#1559 = ORIENTED_EDGE ( 'NONE', *, *, #7403, .F. ) ;
#1560 = CARTESIAN_POINT ( 'NONE',  ( -3.000000000000000000, 22.50000000000000355, 10.00000000000000000 ) ) ;
#1561 = VERTEX_POINT ( 'NONE', #2156 ) ;
#1562 = DIRECTION ( 'NONE',  ( 0.000000000000000000, 0.000000000000000000, -1.000000000000000000 ) ) ;
#1563 = DIRECTION ( 'NONE',  ( -0.000000000000000000, -0.000000000000000000, -1.000000000000000000 ) ) ;
#1564 = CARTESIAN_POINT ( 'NONE',  ( 60.00000000000000000, 7.347880794884118356E-15, -30.00000000000000000 ) ) ;
#1565 = DIRECTION ( 'NONE',  ( 0.000000000000000000, 0.000000000000000000, 1.000000000000000000 ) ) ;
#1566 = CARTESIAN_POINT ( 'NONE',  ( -9.048619709455111959, -15.70011763207404876, 16.29988236792595302 ) ) ;
#1567 = CARTESIAN_POINT ( 'NONE',  ( 5.000000000000000000, -14.14213562373248401, -15.70213562373165850 ) ) ;
#1568 = CARTESIAN_POINT ( 'NONE',  ( 0.000000000000000000, -9.628187502531647418E-13, -19.99999999999950262 ) ) ;
#1569 = ORIENTED_EDGE ( 'NONE', *, *, #3257, .T. ) ;
#1570 = ORIENTED_EDGE ( 'NONE', *, *, #7422, .T. ) ;
#1571 = LINE ( 'NONE', #3781, #2876 ) ;
#1572 = CARTESIAN_POINT ( 'NONE',  ( 26.21170834203229916, 53.97171801779367684, 11.99999999999999645 ) ) ;
#1573 = EDGE_LOOP ( 'NONE', ( #1976, #6178, #6644, #2482 ) ) ;
#1574 = AXIS2_PLACEMENT_3D ( 'NONE', #6606, #24, #5876 ) ;
#1575 = CARTESIAN_POINT ( 'NONE',  ( 2.323800269068097446, 28.49052126930483197, 1.583192244553113914 ) ) ;
#1576 = EDGE_CURVE ( 'NONE', #3936, #672, #8702, .T. ) ;
#1577 = DIRECTION ( 'NONE',  ( 0.000000000000000000, 0.7071067811865479058, -0.7071067811865472397 ) ) ;
#1578 = CYLINDRICAL_SURFACE ( 'NONE', #2575, 1.560000000000000719 ) ;
#1579 = ORIENTED_EDGE ( 'NONE', *, *, #9105, .F. ) ;
#1580 = ORIENTED_EDGE ( 'NONE', *, *, #3127, .F. ) ;
#1581 = DIRECTION ( 'NONE',  ( 6.396792817664419153E-18, 0.9997175446104182850, -0.02376617340079449289 ) ) ;
#1582 = CARTESIAN_POINT ( 'NONE',  ( 0.000000000000000000, 22.50000000000000355, 5.000000000000000000 ) ) ;
#1583 = AXIS2_PLACEMENT_3D ( 'NONE', #1133, #6773, #187 ) ;
#1584 = DIRECTION ( 'NONE',  ( 1.000000000000000000, 0.000000000000000000, 0.000000000000000000 ) ) ;
#1585 = DIRECTION ( 'NONE',  ( -1.000000000000000000, 0.000000000000000000, 0.000000000000000000 ) ) ;
#1586 = AXIS2_PLACEMENT_3D ( 'NONE', #4601, #3875, #7614 ) ;
#1587 = FACE_OUTER_BOUND ( 'NONE', #2085, .T. ) ;
#1588 = DIRECTION ( 'NONE',  ( -0.7071067811865481278, 0.4999999999999994449, 0.4999999999999998890 ) ) ;
#1589 = EDGE_CURVE ( 'NONE', #2537, #2280, #3787, .T. ) ;
#1590 = CARTESIAN_POINT ( 'NONE',  ( 9.048619709455111959, 15.70011763207404876, 16.29988236792595302 ) ) ;
#1591 = CARTESIAN_POINT ( 'NONE',  ( 53.29490495164537833, -30.00000000000000000, -97.50000000000002842 ) ) ;
#1592 = EDGE_LOOP ( 'NONE', ( #4138, #3431, #5308, #1026 ) ) ;
#1593 = ADVANCED_FACE ( 'NONE', ( #8689 ), #2108, .F. ) ;
#1594 =( LENGTH_UNIT ( ) NAMED_UNIT ( * ) SI_UNIT ( .MILLI., .METRE. ) );
#1595 = ADVANCED_FACE ( 'NONE', ( #7291 ), #8399, .F. ) ;
#1596 = ADVANCED_FACE ( 'NONE', ( #3 ), #1796, .F. ) ;
#1597 = EDGE_LOOP ( 'NONE', ( #6253, #4748, #1285, #3156 ) ) ;
#1598 = DIRECTION ( 'NONE',  ( 0.000000000000000000, 0.000000000000000000, 1.000000000000000000 ) ) ;
#1599 = FACE_OUTER_BOUND ( 'NONE', #7856, .T. ) ;
#1600 = CARTESIAN_POINT ( 'NONE',  ( -0.7500000000000000000, 0.7500000000000000000, 1.500000000000000000 ) ) ;
#1601 = CARTESIAN_POINT ( 'NONE',  ( -15.70011763207405231, 9.048619709455117288, 47.70011763207405409 ) ) ;
#1602 = ORIENTED_EDGE ( 'NONE', *, *, #1413, .T. ) ;
#1603 = AXIS2_PLACEMENT_3D ( 'NONE', #2769, #7852, #5107 ) ;
#1604 = ORIENTED_EDGE ( 'NONE', *, *, #9381, .F. ) ;
#1605 = ORIENTED_EDGE ( 'NONE', *, *, #4812, .T. ) ;
#1606 =( NAMED_UNIT ( * ) PLANE_ANGLE_UNIT ( ) SI_UNIT ( $, .RADIAN. ) );
#1607 = EDGE_LOOP ( 'NONE', ( #6203, #4707 ) ) ;
#1608 = CARTESIAN_POINT ( 'NONE',  ( 0.000000000000000000, 0.000000000000000000, 0.000000000000000000 ) ) ;
#1609 = CARTESIAN_POINT ( 'NONE',  ( -53.29490495164537833, 27.56180520566615044, -41.61356529332876875 ) ) ;
#1610 = ADVANCED_FACE ( 'NONE', ( #5285 ), #7583, .F. ) ;
#1611 = CARTESIAN_POINT ( 'NONE',  ( 60.00000000000000000, 29.99999999999999645, -82.50000000000000000 ) ) ;
#1612 = CARTESIAN_POINT ( 'NONE',  ( 0.000000000000000000, 7.653668647302530381, 18.47759065022802716 ) ) ;
#1613 = CARTESIAN_POINT ( 'NONE',  ( 19.62310601229373930, 19.62310601229373930, 26.87436867076457503 ) ) ;
#1614 = AXIS2_PLACEMENT_3D ( 'NONE', #6760, #5504, #4539 ) ;
#1615 = EDGE_CURVE ( 'NONE', #2574, #1684, #9069, .T. ) ;
#1616 = DIRECTION ( 'NONE',  ( 1.000000000000000000, 0.000000000000000000, 0.000000000000000000 ) ) ;
#1617 = LINE ( 'NONE', #5275, #3582 ) ;
#1618 = ORIENTED_EDGE ( 'NONE', *, *, #7580, .T. ) ;
#1619 = ORIENTED_EDGE ( 'NONE', *, *, #8715, .F. ) ;
#1620 = PLANE ( 'NONE',  #7629 ) ;
#1621 = LINE ( 'NONE', #2398, #5183 ) ;
#1622 = ORIENTED_EDGE ( 'NONE', *, *, #1720, .F. ) ;
#1623 = AXIS2_PLACEMENT_3D ( 'NONE', #54, #1533, #2256 ) ;
#1624 = CARTESIAN_POINT ( 'NONE',  ( 2.651740589948411664, 28.40946940741335069, 1.531087476194299413 ) ) ;
#1625 = SHAPE_REPRESENTATION ( '2-Bush', ( #1614 ), #7287 ) ;
#1626 = CARTESIAN_POINT ( 'NONE',  ( -18.50000000000001776, 0.000000000000000000, 0.000000000000000000 ) ) ;
#1627 = UNCERTAINTY_MEASURE_WITH_UNIT (LENGTH_MEASURE( 1.000000000000000082E-05 ), #4150, 'distance_accuracy_value', 'NONE');
#1628 = CARTESIAN_POINT ( 'NONE',  ( -4.703319286132083832, -17.49999999999999645, 49.50000000000000000 ) ) ;
#1629 = CIRCLE ( 'NONE', #3005, 3.000000000000002665 ) ;
#1630 = ORIENTED_EDGE ( 'NONE', *, *, #4418, .F. ) ;
#1631 = ORIENTED_EDGE ( 'NONE', *, *, #2262, .F. ) ;
#1632 = SHAPE_DEFINITION_REPRESENTATION ( #8161, #3963 ) ;
#1633 = ADVANCED_FACE ( 'NONE', ( #6008 ), #6918, .T. ) ;
#1634 = DIRECTION ( 'NONE',  ( -1.000000000000000000, 0.000000000000000000, 0.000000000000000000 ) ) ;
#1635 = CARTESIAN_POINT ( 'NONE',  ( -48.15955140082797925, -36.58521010404104601, -10.14640895491554140 ) ) ;
#1636 = VECTOR ( 'NONE', #8439, 1000.000000000000000 ) ;
#1637 = VECTOR ( 'NONE', #8391, 1000.000000000000000 ) ;
#1638 = CARTESIAN_POINT ( 'NONE',  ( 0.000000000000000000, 7.653668647300657213, -18.47759065022568237 ) ) ;
#1639 = ADVANCED_FACE ( 'NONE', ( #1820 ), #999, .F. ) ;
#1640 = FACE_OUTER_BOUND ( 'NONE', #7306, .T. ) ;
#1641 = DIRECTION ( 'NONE',  ( 0.000000000000000000, 0.000000000000000000, -1.000000000000000000 ) ) ;
#1642 = CARTESIAN_POINT ( 'NONE',  ( 0.000000000000000000, 0.000000000000000000, 27.50000000000000355 ) ) ;
#1643 = CARTESIAN_POINT ( 'NONE',  ( -16.50000000000000000, 7.347880794884122694E-16, 5.000000000000000000 ) ) ;
#1644 = CLOSED_SHELL ( 'NONE', ( #8760, #7621, #5555, #5827, #927, #4656, #7916, #824, #6704, #6175, #2946, #7723, #2782, #8654, #7705, #1610, #2011, #3314, #8933, #6967, #3771, #407, #1416, #8175, #7328, #7348, #2665, #2714, #3972, #3510, #1510, #534, #9108, #6120, #3001, #6533, #1757, #7842, #7935, #9358, #2352, #3179, #4532, #9330, #5320, #2830, #6255, #8721, #7227, #5933, #8029, #4759, #2549, #125, #3190, #8065, #2618, #253, #4658, #4012, #4843, #1235, #9235, #6342, #6419, #5736, #2239, #1639, #3706, #7040, #2244, #423, #9312, #1139, #2446, #3219, #1181, #9054, #1143, #4999 ) ) ;
#1645 = ORIENTED_EDGE ( 'NONE', *, *, #9118, .F. ) ;
#1646 = DIRECTION ( 'NONE',  ( -1.000000000000000000, 0.000000000000000000, 0.000000000000000000 ) ) ;
#1647 = ORIENTED_EDGE ( 'NONE', *, *, #1717, .F. ) ;
#1648 = AXIS2_PLACEMENT_3D ( 'NONE', #5972, #3802, #6600 ) ;
#1649 = DIRECTION ( 'NONE',  ( -0.000000000000000000, 1.000000000000000000, 0.000000000000000000 ) ) ;
#1650 = CARTESIAN_POINT ( 'NONE',  ( 4.000000000000000000, -7.653668647303860872, -18.47759065022490432 ) ) ;
#1651 = AXIS2_PLACEMENT_3D ( 'NONE', #6202, #8402, #1769 ) ;
#1652 = AXIS2_PLACEMENT_3D ( 'NONE', #165, #4477, #2373 ) ;
#1653 = DIRECTION ( 'NONE',  ( 0.000000000000000000, 0.000000000000000000, 1.000000000000000000 ) ) ;
#1654 = DIRECTION ( 'NONE',  ( 0.000000000000000000, 0.000000000000000000, -1.000000000000000000 ) ) ;
#1655 = AXIS2_PLACEMENT_3D ( 'NONE', #7536, #949, #3883 ) ;
#1656 = VERTEX_POINT ( 'NONE', #8264 ) ;
#1657 = ORIENTED_EDGE ( 'NONE', *, *, #7827, .F. ) ;
#1658 = ORIENTED_EDGE ( 'NONE', *, *, #7044, .T. ) ;
#1659 = ORIENTED_EDGE ( 'NONE', *, *, #1359, .T. ) ;
#1660 = CARTESIAN_POINT ( 'NONE',  ( 6.000000000000000888, 7.347880794884120722E-16, 4.000000000000000000 ) ) ;
#1661 = EDGE_CURVE ( 'NONE', #7899, #5896, #1307, .T. ) ;
#1662 = DIRECTION ( 'NONE',  ( 0.000000000000000000, 1.000000000000000000, 0.000000000000000000 ) ) ;
#1663 = EDGE_CURVE ( 'NONE', #5576, #6611, #1090, .T. ) ;
#1664 = DIRECTION ( 'NONE',  ( 0.000000000000000000, 0.000000000000000000, 1.000000000000000000 ) ) ;
#1665 = VECTOR ( 'NONE', #2243, 1000.000000000000000 ) ;
#1666 = CARTESIAN_POINT ( 'NONE',  ( 0.000000000000000000, 0.000000000000000000, 0.000000000000000000 ) ) ;
#1667 = PLANE ( 'NONE',  #6673 ) ;
#1668 = CARTESIAN_POINT ( 'NONE',  ( -37.00000000000000711, 15.90990257669733943, -51.09009742330271564 ) ) ;
#1669 = ORIENTED_EDGE ( 'NONE', *, *, #4554, .T. ) ;
#1670 = ORIENTED_EDGE ( 'NONE', *, *, #7859, .T. ) ;
#1671 = DIRECTION ( 'NONE',  ( 0.000000000000000000, 0.000000000000000000, 1.000000000000000000 ) ) ;
#1672 = CIRCLE ( 'NONE', #2752, 26.99999999999997868 ) ;
#1673 = VERTEX_POINT ( 'NONE', #6107 ) ;
#1674 = LINE ( 'NONE', #6866, #6200 ) ;
#1675 = AXIS2_PLACEMENT_3D ( 'NONE', #3606, #158, #58 ) ;
#1676 = CARTESIAN_POINT ( 'NONE',  ( 17.49999999999999645, 4.703319286132083832, 49.50000000000000000 ) ) ;
#1677 = VERTEX_POINT ( 'NONE', #8306 ) ;
#1678 = APPLICATION_CONTEXT ( 'automotive_design' ) ;
#1679 = DIRECTION ( 'NONE',  ( 0.000000000000000000, 0.000000000000000000, 1.000000000000000000 ) ) ;
#1680 = AXIS2_PLACEMENT_3D ( 'NONE', #7354, #8080, #4431 ) ;
#1681 = DIRECTION ( 'NONE',  ( -1.000000000000000000, -0.000000000000000000, -0.000000000000000000 ) ) ;
#1682 = CARTESIAN_POINT ( 'NONE',  ( 61.20398523554579384, 8.188417774577869679, -89.59091971609970528 ) ) ;
#1683 = ORIENTED_EDGE ( 'NONE', *, *, #5010, .T. ) ;
#1684 = VERTEX_POINT ( 'NONE', #4034 ) ;
#1685 = DIRECTION ( 'NONE',  ( -1.080252097649406280E-16, -0.9911323735125173728, 0.1328782080532535659 ) ) ;
#1686 = DIRECTION ( 'NONE',  ( -0.000000000000000000, -0.000000000000000000, 1.000000000000000000 ) ) ;
#1687 =( BOUNDED_CURVE ( )  B_SPLINE_CURVE ( 3, ( #5215, #77, #2999, #5935 ),
 .UNSPECIFIED., .F., .T. ) 
 B_SPLINE_CURVE_WITH_KNOTS ( ( 4, 4 ),
 ( 3.141592653589793116, 3.926990816987241395 ),
 .UNSPECIFIED. ) 
 CURVE ( )  GEOMETRIC_REPRESENTATION_ITEM ( )  RATIONAL_B_SPLINE_CURVE ( ( 1.000000000000000000, 0.9492530216741911220, 0.9492530216741911220, 1.000000000000000000 ) ) 
 REPRESENTATION_ITEM ( '' )  );
#1688 = CYLINDRICAL_SURFACE ( 'NONE', #1187, 6.000000000000001776 ) ;
#1689 = CARTESIAN_POINT ( 'NONE',  ( -53.29490495164537833, -15.90990257669733943, -51.09009742330271564 ) ) ;
#1690 = CARTESIAN_POINT ( 'NONE',  ( 13.50000000000000178, 0.000000000000000000, 28.50000000000000355 ) ) ;
#1691 = DIRECTION ( 'NONE',  ( 0.000000000000000000, -0.7071067811865479058, 0.7071067811865472397 ) ) ;
#1692 = ORIENTED_EDGE ( 'NONE', *, *, #6006, .F. ) ;
#1693 = CYLINDRICAL_SURFACE ( 'NONE', #9301, 0.7500000000017874591 ) ;
#1694 = VERTEX_POINT ( 'NONE', #909 ) ;
#1695 = CARTESIAN_POINT ( 'NONE',  ( 12.50000000000000000, 1.530808498934191127E-15, 50.00000000000000000 ) ) ;
#1696 = CARTESIAN_POINT ( 'NONE',  ( 0.000000000000000000, 0.000000000000000000, 63.00000000000002842 ) ) ;
#1697 = DIRECTION ( 'NONE',  ( -1.000000000000000000, 0.000000000000000000, 0.000000000000000000 ) ) ;
#1698 = CARTESIAN_POINT ( 'NONE',  ( 53.29490495164537833, 15.90990257669733943, -51.09009742330271564 ) ) ;
#1699 = VERTEX_POINT ( 'NONE', #6966 ) ;
#1700 = EDGE_LOOP ( 'NONE', ( #5140, #6310, #1016, #5227 ) ) ;
#1701 = VERTEX_POINT ( 'NONE', #375 ) ;
#1702 = EDGE_LOOP ( 'NONE', ( #3929, #6032 ) ) ;
#1703 = ADVANCED_FACE ( 'NONE', ( #8926 ), #4705, .T. ) ;
#1704 = DIRECTION ( 'NONE',  ( 0.000000000000000000, 0.000000000000000000, 1.000000000000000000 ) ) ;
#1705 = DIRECTION ( 'NONE',  ( 1.000000000000000000, -0.000000000000000000, -0.000000000000000000 ) ) ;
#1706 = CIRCLE ( 'NONE', #5396, 3.000000000000002665 ) ;
#1707 = FACE_OUTER_BOUND ( 'NONE', #670, .T. ) ;
#1708 = CARTESIAN_POINT ( 'NONE',  ( -6.000000000000000888, 22.50000000000000355, 5.000000000000000000 ) ) ;
#1709 = DIRECTION ( 'NONE',  ( 0.000000000000000000, 0.000000000000000000, -1.000000000000000000 ) ) ;
#1710 = CARTESIAN_POINT ( 'NONE',  ( 0.000000000000000000, 0.000000000000000000, -22.00000000000000711 ) ) ;
#1711 = DIRECTION ( 'NONE',  ( -0.7071067811865505703, -0.7071067811865444641, -0.000000000000000000 ) ) ;
#1712 = EDGE_LOOP ( 'NONE', ( #3856, #4 ) ) ;
#1713 = EDGE_CURVE ( 'NONE', #3455, #7998, #2734, .T. ) ;
#1714 = ORIENTED_EDGE ( 'NONE', *, *, #1049, .T. ) ;
#1715 = CARTESIAN_POINT ( 'NONE',  ( 0.000000000000000000, 0.000000000000000000, 11.99999999999999645 ) ) ;
#1716 = ORIENTED_EDGE ( 'NONE', *, *, #2452, .T. ) ;
#1717 = EDGE_CURVE ( 'NONE', #8845, #4404, #3137, .T. ) ;
#1718 = FACE_BOUND ( 'NONE', #7249, .T. ) ;
#1719 = EDGE_CURVE ( 'NONE', #4290, #7899, #6237, .T. ) ;
#1720 = EDGE_CURVE ( 'NONE', #3965, #6890, #421, .T. ) ;
#1721 = ORIENTED_EDGE ( 'NONE', *, *, #9169, .T. ) ;
#1722 = CIRCLE ( 'NONE', #8611, 8.000000000000021316 ) ;
#1723 = CARTESIAN_POINT ( 'NONE',  ( 3.600085285568724203, 28.11218154377481682, 1.339973849569531472 ) ) ;
#1724 = FACE_OUTER_BOUND ( 'NONE', #2138, .T. ) ;
#1725 = CARTESIAN_POINT ( 'NONE',  ( 0.000000000000000000, 0.000000000000000000, 50.00000000000000000 ) ) ;
#1726 = ORIENTED_EDGE ( 'NONE', *, *, #4554, .F. ) ;
#1727 = EDGE_LOOP ( 'NONE', ( #8694, #283, #6075, #2298 ) ) ;
#1728 = APPLICATION_PROTOCOL_DEFINITION ( 'draft international standard', 'automotive_design', 1998, #996 ) ;
#1729 = AXIS2_PLACEMENT_3D ( 'NONE', #1837, #874, #1204 ) ;
#1730 = CARTESIAN_POINT ( 'NONE',  ( 0.7500000000000000000, 2.749999999999995559, 0.000000000000000000 ) ) ;
#1731 = EDGE_CURVE ( 'NONE', #7912, #7789, #3395, .T. ) ;
#1732 = CARTESIAN_POINT ( 'NONE',  ( -0.7500000000000000000, -2.749999999999995559, 0.000000000000000000 ) ) ;
#1733 = AXIS2_PLACEMENT_3D ( 'NONE', #3285, #8331, #2387 ) ;
#1734 = PLANE ( 'NONE',  #8430 ) ;
#1735 = EDGE_CURVE ( 'NONE', #4149, #9366, #8587, .T. ) ;
#1736 = DIRECTION ( 'NONE',  ( -0.000000000000000000, -0.000000000000000000, 1.000000000000000000 ) ) ;
#1737 = ORIENTED_EDGE ( 'NONE', *, *, #2850, .T. ) ;
#1738 = VERTEX_POINT ( 'NONE', #8543 ) ;
#1739 = FACE_OUTER_BOUND ( 'NONE', #3588, .T. ) ;
#1740 = DIRECTION ( 'NONE',  ( 0.000000000000000000, 0.000000000000000000, -1.000000000000000000 ) ) ;
#1741 = VECTOR ( 'NONE', #2630, 1000.000000000000000 ) ;
#1742 = PLANE ( 'NONE',  #9196 ) ;
#1743 = CARTESIAN_POINT ( 'NONE',  ( 60.00000000000000000, 29.99999999999999645, -82.50000000000000000 ) ) ;
#1744 = ORIENTED_EDGE ( 'NONE', *, *, #325, .T. ) ;
#1745 = ORIENTED_EDGE ( 'NONE', *, *, #598, .F. ) ;
#1746 = ORIENTED_EDGE ( 'NONE', *, *, #3218, .T. ) ;
#1747 =( LENGTH_UNIT ( ) NAMED_UNIT ( * ) SI_UNIT ( .MILLI., .METRE. ) );
#1748 = ORIENTED_EDGE ( 'NONE', *, *, #4956, .F. ) ;
#1749 = CARTESIAN_POINT ( 'NONE',  ( -14.49999999999995381, 9.797174393178884822E-16, 0.000000000000000000 ) ) ;
#1750 = LINE ( 'NONE', #980, #8019 ) ;
#1751 = DIRECTION ( 'NONE',  ( -1.000000000000000000, 0.000000000000000000, 0.000000000000000000 ) ) ;
#1752 = EDGE_CURVE ( 'NONE', #3888, #2481, #7518, .T. ) ;
#1753 = AXIS2_PLACEMENT_3D ( 'NONE', #2402, #1681, #908 ) ;
#1754 = DIRECTION ( 'NONE',  ( -1.000000000000000000, -0.000000000000000000, -0.000000000000000000 ) ) ;
#1755 = CONICAL_SURFACE ( 'NONE', #3437, 22.50000000000000000, 0.7853981633974447263 ) ;
#1756 = CARTESIAN_POINT ( 'NONE',  ( 0.000000000000000000, 22.50000000000000355, 5.000000000000000000 ) ) ;
#1757 = ADVANCED_FACE ( 'NONE', ( #7008 ), #2738, .T. ) ;
#1758 = CARTESIAN_POINT ( 'NONE',  ( 0.000000000000000000, 0.000000000000000000, 48.00000000000036948 ) ) ;
#1759 = EDGE_LOOP ( 'NONE', ( #243, #1379, #8307, #3835 ) ) ;
#1760 = CIRCLE ( 'NONE', #1913, 3.000000000000002665 ) ;
#1761 = ORIENTED_EDGE ( 'NONE', *, *, #4826, .F. ) ;
#1762 = DIRECTION ( 'NONE',  ( 0.000000000000000000, 0.000000000000000000, -1.000000000000000000 ) ) ;
#1763 = ORIENTED_EDGE ( 'NONE', *, *, #7594, .F. ) ;
#1764 = DIRECTION ( 'NONE',  ( 1.000000000000000000, 0.000000000000000000, -0.000000000000000000 ) ) ;
#1765 = CARTESIAN_POINT ( 'NONE',  ( 3.000000000000000444, 3.673940397442060361E-16, 21.00000000000000000 ) ) ;
#1766 = VERTEX_POINT ( 'NONE', #4269 ) ;
#1767 = DIRECTION ( 'NONE',  ( 1.000000000000000000, 0.000000000000000000, 0.000000000000000000 ) ) ;
#1768 = CYLINDRICAL_SURFACE ( 'NONE', #8201, 11.00000000000000000 ) ;
#1769 = DIRECTION ( 'NONE',  ( -1.000000000000000000, 0.000000000000000000, 0.000000000000000000 ) ) ;
#1770 = ORIENTED_EDGE ( 'NONE', *, *, #3518, .F. ) ;
#1771 = EDGE_LOOP ( 'NONE', ( #4684, #5251, #5302, #6564 ) ) ;
#1772 = AXIS2_PLACEMENT_3D ( 'NONE', #8072, #8213, #3696 ) ;
#1773 = ITEM_DEFINED_TRANSFORMATION ( 'NONE', 'NONE', #4222,  #1614 ) ;
#1774 = FACE_OUTER_BOUND ( 'NONE', #7836, .T. ) ;
#1775 = ADVANCED_FACE ( 'NONE', ( #7867 ), #2596, .F. ) ;
#1776 = CARTESIAN_POINT ( 'NONE',  ( 3.000000000000156763, -22.50000000000000355, 5.000000000000000000 ) ) ;
#1777 = AXIS2_PLACEMENT_3D ( 'NONE', #914, #1686, #7772 ) ;
#1778 = CARTESIAN_POINT ( 'NONE',  ( 0.000000000000000000, 0.000000000000000000, 25.00000000000000000 ) ) ;
#1779 = DIRECTION ( 'NONE',  ( 0.000000000000000000, 0.000000000000000000, 1.000000000000000000 ) ) ;
#1780 = CARTESIAN_POINT ( 'NONE',  ( -28.48969330601477168, 2.327370969396575617, 1.582659982438082036 ) ) ;
#1781 = EDGE_LOOP ( 'NONE', ( #4751, #7391, #2761, #5715, #4013 ) ) ;
#1782 = LINE ( 'NONE', #4723, #3333 ) ;
#1783 = ORIENTED_EDGE ( 'NONE', *, *, #3897, .F. ) ;
#1784 = AXIS2_PLACEMENT_3D ( 'NONE', #3868, #8288, #2626 ) ;
#1785 = CARTESIAN_POINT ( 'NONE',  ( 27.00000000000000000, 43.00000000000000000, 11.99999999999999645 ) ) ;
#1786 = DIRECTION ( 'NONE',  ( -0.000000000000000000, -0.000000000000000000, -1.000000000000000000 ) ) ;
#1787 = LINE ( 'NONE', #6276, #6440 ) ;
#1788 = LINE ( 'NONE', #2568, #7083 ) ;
#1789 = VECTOR ( 'NONE', #5153, 1000.000000000000000 ) ;
#1790 = ORIENTED_EDGE ( 'NONE', *, *, #6654, .F. ) ;
#1791 =( BOUNDED_CURVE ( )  B_SPLINE_CURVE ( 3, ( #7370, #2997, #5112, #7273 ),
 .UNSPECIFIED., .F., .F. ) 
 B_SPLINE_CURVE_WITH_KNOTS ( ( 4, 4 ),
 ( 0.000000000000000000, 0.4772783968222097384 ),
 .UNSPECIFIED. ) 
 CURVE ( )  GEOMETRIC_REPRESENTATION_ITEM ( )  RATIONAL_B_SPLINE_CURVE ( ( 1.000000000000000000, 0.9811070276743185659, 0.9811070276743185659, 1.000000000000000000 ) ) 
 REPRESENTATION_ITEM ( '' )  );
#1792 = APPLICATION_CONTEXT ( 'automotive_design' ) ;
#1793 = ORIENTED_EDGE ( 'NONE', *, *, #2121, .F. ) ;
#1794 = ORIENTED_EDGE ( 'NONE', *, *, #7444, .T. ) ;
#1795 = ORIENTED_EDGE ( 'NONE', *, *, #8757, .F. ) ;
#1796 = CONICAL_SURFACE ( 'NONE', #5487, 6.000000000000001776, 0.7853981633974431720 ) ;
#1797 = CARTESIAN_POINT ( 'NONE',  ( 17.50000000000000355, 0.000000000000000000, 63.00000000000002842 ) ) ;
#1798 = CIRCLE ( 'NONE', #7321, 7.250000000000002665 ) ;
#1799 = DIRECTION ( 'NONE',  ( -1.000000000000000000, 0.000000000000000000, 0.000000000000000000 ) ) ;
#1800 = AXIS2_PLACEMENT_3D ( 'NONE', #2797, #9319, #7028 ) ;
#1801 = CARTESIAN_POINT ( 'NONE',  ( 11.96410161513786008, 1.465179874765226021E-15, 50.00000000000000000 ) ) ;
#1802 = VECTOR ( 'NONE', #2059, 1000.000000000000000 ) ;
#1803 = CARTESIAN_POINT ( 'NONE',  ( 27.81412668510617436, 2.815004828058581765, 0.9535900900804922253 ) ) ;
#1804 = CIRCLE ( 'NONE', #9164, 0.7500000000012114754 ) ;
#1805 = CARTESIAN_POINT ( 'NONE',  ( 28.68405123480337693, -1.339801352072190310, 1.707604365230744659 ) ) ;
#1806 = EDGE_CURVE ( 'NONE', #5838, #9262, #7057, .T. ) ;
#1807 = AXIS2_PLACEMENT_3D ( 'NONE', #9210, #8502, #2649 ) ;
#1808 = ORIENTED_EDGE ( 'NONE', *, *, #952, .T. ) ;
#1809 = VERTEX_POINT ( 'NONE', #5575 ) ;
#1810 = LINE ( 'NONE', #7527, #8521 ) ;
#1811 = ORIENTED_EDGE ( 'NONE', *, *, #5416, .F. ) ;
#1812 = DIRECTION ( 'NONE',  ( -0.7071067811865460184, -0.7071067811865489050, -9.185433182841358520E-17 ) ) ;
#1813 = PRESENTATION_LAYER_ASSIGNMENT (  '', '', ( #6579 ) ) ;
#1814 = EDGE_LOOP ( 'NONE', ( #8597, #6397, #7503, #8647 ) ) ;
#1815 = ADVANCED_FACE ( 'NONE', ( #9204 ), #8454, .F. ) ;
#1816 = CARTESIAN_POINT ( 'NONE',  ( 26.21170834203226718, -53.97171801779368394, -2.612255525622730001 ) ) ;
#1817 = CIRCLE ( 'NONE', #7184, 2.999999999999999112 ) ;
#1818 = CARTESIAN_POINT ( 'NONE',  ( 52.86930915046634993, -28.38475884032111907, -81.18159060786260284 ) ) ;
#1819 = VECTOR ( 'NONE', #8768, 1000.000000000000000 ) ;
#1820 = FACE_OUTER_BOUND ( 'NONE', #211, .T. ) ;
#1821 = EDGE_LOOP ( 'NONE', ( #6919, #5503 ) ) ;
#1822 = CIRCLE ( 'NONE', #3356, 1.560000000001466436 ) ;
#1823 = ORIENTED_EDGE ( 'NONE', *, *, #3528, .T. ) ;
#1824 = EDGE_CURVE ( 'NONE', #1107, #1266, #7910, .T. ) ;
#1825 = AXIS2_PLACEMENT_3D ( 'NONE', #7134, #554, #4071 ) ;
#1826 = LINE ( 'NONE', #4616, #7164 ) ;
#1827 = PLANE ( 'NONE',  #381 ) ;
#1828 = CARTESIAN_POINT ( 'NONE',  ( -37.00000000000000000, 30.00000000000000000, -95.00000000000000000 ) ) ;
#1829 = CARTESIAN_POINT ( 'NONE',  ( 30.00000000000000000, 3.673940397442059178E-15, 10.00000000000000000 ) ) ;
#1830 = CARTESIAN_POINT ( 'NONE',  ( 0.000000000000000000, 0.000000000000000000, 27.50000000000000355 ) ) ;
#1831 = EDGE_CURVE ( 'NONE', #849, #2124, #7034, .T. ) ;
#1832 = VERTEX_POINT ( 'NONE', #6437 ) ;
#1833 = EDGE_CURVE ( 'NONE', #3385, #8070, #6412, .T. ) ;
#1834 = CARTESIAN_POINT ( 'NONE',  ( -27.00000000000000000, 43.00000000000000000, 11.99999999999999645 ) ) ;
#1835 = VERTEX_POINT ( 'NONE', #6524 ) ;
#1836 = EDGE_CURVE ( 'NONE', #5958, #6044, #9444, .T. ) ;
#1837 = CARTESIAN_POINT ( 'NONE',  ( 0.000000000000000000, -14.14213562373112154, 14.14213562373418220 ) ) ;
#1838 = EDGE_CURVE ( 'NONE', #2635, #2331, #2095, .T. ) ;
#1839 = ADVANCED_FACE ( 'NONE', ( #659 ), #8820, .F. ) ;
#1840 = CARTESIAN_POINT ( 'NONE',  ( 0.000000000000000000, 14.14213562373112154, -14.14213562373077870 ) ) ;
#1841 = CARTESIAN_POINT ( 'NONE',  ( 32.00000000000000711, -34.99999999999999289, 64.00000000000000000 ) ) ;
#1842 = AXIS2_PLACEMENT_3D ( 'NONE', #4187, #7112, #3459 ) ;
#1843 = CARTESIAN_POINT ( 'NONE',  ( 48.15955140082798636, -36.58521010404105311, -10.14640895491553962 ) ) ;
#1844 = ORIENTED_EDGE ( 'NONE', *, *, #5942, .T. ) ;
#1845 = EDGE_LOOP ( 'NONE', ( #6698, #6887, #2168, #9187 ) ) ;
#1846 = DIRECTION ( 'NONE',  ( 0.000000000000000000, 0.000000000000000000, 1.000000000000000000 ) ) ;
#1847 = ORIENTED_EDGE ( 'NONE', *, *, #5753, .F. ) ;
#1848 = EDGE_CURVE ( 'NONE', #7733, #3876, #6726, .T. ) ;
#1849 = CARTESIAN_POINT ( 'NONE',  ( -17.50000000000000355, 2.143131898507868643E-15, 63.00000000000002842 ) ) ;
#1850 = EDGE_CURVE ( 'NONE', #9368, #334, #8406, .T. ) ;
#1851 = CYLINDRICAL_SURFACE ( 'NONE', #1476, 6.000000000000000888 ) ;
#1852 = AXIS2_PLACEMENT_3D ( 'NONE', #7055, #2684, #3393 ) ;
#1853 = EDGE_CURVE ( 'NONE', #7405, #5068, #9308, .T. ) ;
#1854 = LINE ( 'NONE', #1801, #5698 ) ;
#1855 = CARTESIAN_POINT ( 'NONE',  ( -43.18827341296425715, 42.33902489539482872, -7.653089211995568242 ) ) ;
#1856 = DIRECTION ( 'NONE',  ( -1.000000000000000000, -0.000000000000000000, -0.000000000000000000 ) ) ;
#1857 = VERTEX_POINT ( 'NONE', #7377 ) ;
#1858 = ORIENTED_EDGE ( 'NONE', *, *, #814, .F. ) ;
#1859 = FACE_OUTER_BOUND ( 'NONE', #4732, .T. ) ;
#1860 = CIRCLE ( 'NONE', #2634, 0.7499999999989250821 ) ;
#1861 = EDGE_LOOP ( 'NONE', ( #1342, #1182, #2045, #1530 ) ) ;
#1862 = PLANE ( 'NONE',  #3273 ) ;
#1863 = CARTESIAN_POINT ( 'NONE',  ( 27.00000000000000355, 35.00000000000000000, 59.00000000000000000 ) ) ;
#1864 = ORIENTED_EDGE ( 'NONE', *, *, #4032, .F. ) ;
#1865 = DIRECTION ( 'NONE',  ( 1.000000000000000000, 0.000000000000000000, 0.000000000000000000 ) ) ;
#1866 = CARTESIAN_POINT ( 'NONE',  ( -26.99999999999998934, -34.99999999999999289, 5.000000000000004441 ) ) ;
#1867 = DIRECTION ( 'NONE',  ( -0.000000000000000000, -0.000000000000000000, -1.000000000000000000 ) ) ;
#1868 = ORIENTED_EDGE ( 'NONE', *, *, #7827, .T. ) ;
#1869 = ORIENTED_EDGE ( 'NONE', *, *, #349, .F. ) ;
#1870 = AXIS2_PLACEMENT_3D ( 'NONE', #6510, #2134, #5835 ) ;
#1871 = ITEM_DEFINED_TRANSFORMATION ( 'NONE', 'NONE', #7600,  #1614 ) ;
#1872 = CARTESIAN_POINT ( 'NONE',  ( 0.000000000000000000, -18.47759065022712832, 7.653668647304757044 ) ) ;
#1873 = AXIS2_PLACEMENT_3D ( 'NONE', #5970, #7353, #2317 ) ;
#1874 = DIRECTION ( 'NONE',  ( 0.000000000000000000, 0.000000000000000000, 1.000000000000000000 ) ) ;
#1875 = FILL_AREA_STYLE ('',( #9122 ) ) ;
#1876 = CARTESIAN_POINT ( 'NONE',  ( -51.96152422706632734, 30.00000000000000000, -80.85015119857381194 ) ) ;
#1877 = DIRECTION ( 'NONE',  ( 0.000000000000000000, 0.000000000000000000, -1.000000000000000000 ) ) ;
#1878 = VECTOR ( 'NONE', #3275, 1000.000000000000000 ) ;
#1879 = ORIENTED_EDGE ( 'NONE', *, *, #1663, .T. ) ;
#1880 = DIRECTION ( 'NONE',  ( -0.000000000000000000, -0.000000000000000000, -1.000000000000000000 ) ) ;
#1881 = ORIENTED_EDGE ( 'NONE', *, *, #3809, .T. ) ;
#1882 = LINE ( 'NONE', #5731, #5573 ) ;
#1883 = LINE ( 'NONE', #7747, #4871 ) ;
#1884 = AXIS2_PLACEMENT_3D ( 'NONE', #7079, #4868, #7803 ) ;
#1885 = CYLINDRICAL_SURFACE ( 'NONE', #2072, 17.50000000000000000 ) ;
#1886 = LINE ( 'NONE', #6317, #638 ) ;
#1887 = ADVANCED_FACE ( 'NONE', ( #2147 ), #4497, .F. ) ;
#1888 = CARTESIAN_POINT ( 'NONE',  ( -30.00000000000000000, 3.673940397442059178E-15, 2.999999999999999112 ) ) ;
#1889 = EDGE_CURVE ( 'NONE', #4158, #7322, #3798, .T. ) ;
#1890 = VERTEX_POINT ( 'NONE', #8775 ) ;
#1891 = ORIENTED_EDGE ( 'NONE', *, *, #889, .T. ) ;
#1892 = DIRECTION ( 'NONE',  ( 9.801187639268983503E-17, -0.9997175446104182850, 0.02376617340079571414 ) ) ;
#1893 = ORIENTED_EDGE ( 'NONE', *, *, #7002, .T. ) ;
#1894 = FACE_BOUND ( 'NONE', #6267, .T. ) ;
#1895 = VECTOR ( 'NONE', #8504, 1000.000000000000000 ) ;
#1896 = CARTESIAN_POINT ( 'NONE',  ( 0.000000000000000000, 0.000000000000000000, 2.999999999999999112 ) ) ;
#1897 = CARTESIAN_POINT ( 'NONE',  ( 0.000000000000000000, -18.47759065022790637, -6.903668647298391470 ) ) ;
#1898 = CARTESIAN_POINT ( 'NONE',  ( 28.40898306695985198, 1.062480114424067201, 1.428075945201422670 ) ) ;
#1899 = CARTESIAN_POINT ( 'NONE',  ( 0.000000000000000000, 0.000000000000000000, 0.000000000000000000 ) ) ;
#1900 = VERTEX_POINT ( 'NONE', #5078 ) ;
#1901 = ORIENTED_EDGE ( 'NONE', *, *, #2046, .T. ) ;
#1902 = ADVANCED_FACE ( 'NONE', ( #5122 ), #612, .F. ) ;
#1903 = CARTESIAN_POINT ( 'NONE',  ( 27.00000000000000000, -43.00000000000000000, -25.00000000000000000 ) ) ;
#1904 = VERTEX_POINT ( 'NONE', #6482 ) ;
#1905 = EDGE_CURVE ( 'NONE', #9340, #1115, #2236, .T. ) ;
#1906 = CARTESIAN_POINT ( 'NONE',  ( 4.000000000000000000, -14.14213562373248401, -12.58213562372718641 ) ) ;
#1907 = AXIS2_PLACEMENT_3D ( 'NONE', #5134, #1477, #2304 ) ;
#1908 = CARTESIAN_POINT ( 'NONE',  ( 27.00000000000000000, 43.00000000000000000, 25.00000000000000000 ) ) ;
#1909 = EDGE_LOOP ( 'NONE', ( #9309, #2793, #5362, #635 ) ) ;
#1910 = DIRECTION ( 'NONE',  ( -1.000000000000000000, -0.000000000000000000, -0.000000000000000000 ) ) ;
#1911 = CARTESIAN_POINT ( 'NONE',  ( -26.02777777777775370, 7.180166011355047395, 0.000000000000000000 ) ) ;
#1912 = EDGE_CURVE ( 'NONE', #1900, #9366, #1804, .T. ) ;
#1913 = AXIS2_PLACEMENT_3D ( 'NONE', #6620, #1376, #3584 ) ;
#1914 = DIRECTION ( 'NONE',  ( 0.000000000000000000, 0.000000000000000000, 1.000000000000000000 ) ) ;
#1915 = DIRECTION ( 'NONE',  ( -0.7071067811865470176, 0.000000000000000000, 0.7071067811865481278 ) ) ;
#1916 = EDGE_LOOP ( 'NONE', ( #6537, #5907, #4701, #9273 ) ) ;
#1917 = AXIS2_PLACEMENT_3D ( 'NONE', #2531, #4875, #6144 ) ;
#1918 = ORIENTED_EDGE ( 'NONE', *, *, #6530, .F. ) ;
#1919 = CARTESIAN_POINT ( 'NONE',  ( 14.49999999999998579, 0.000000000000000000, 0.000000000000000000 ) ) ;
#1920 = PLANE ( 'NONE',  #8048 ) ;
#1921 = FACE_OUTER_BOUND ( 'NONE', #1154, .T. ) ;
#1922 = DIRECTION ( 'NONE',  ( 1.000000000000000000, 0.000000000000000000, 0.000000000000000000 ) ) ;
#1923 = DIRECTION ( 'NONE',  ( -0.7071067811865494601, 0.000000000000000000, -0.7071067811865455743 ) ) ;
#1924 = ORIENTED_EDGE ( 'NONE', *, *, #1294, .T. ) ;
#1925 = EDGE_CURVE ( 'NONE', #8795, #9218, #5033, .T. ) ;
#1926 = ORIENTED_EDGE ( 'NONE', *, *, #156, .T. ) ;
#1927 = ORIENTED_EDGE ( 'NONE', *, *, #2427, .T. ) ;
#1928 = DIRECTION ( 'NONE',  ( 0.000000000000000000, -1.000000000000000000, 0.000000000000000000 ) ) ;
#1929 = CARTESIAN_POINT ( 'NONE',  ( 0.000000000000000000, 0.000000000000000000, 4.000000000000000000 ) ) ;
#1930 = AXIS2_PLACEMENT_3D ( 'NONE', #6321, #8, #1939 ) ;
#1931 = ADVANCED_FACE ( 'NONE', ( #2825 ), #7331, .T. ) ;
#1932 = CARTESIAN_POINT ( 'NONE',  ( 3.000000000000000000, 22.50000000000000355, 10.00000000000000000 ) ) ;
#1933 = SHAPE_REPRESENTATION ( 'MAT-017', ( #5310, #1465, #4222, #7138, #3919, #7907, #2225, #6083, #1930, #2702, #8530, #2993, #7600, #2079, #4383, #248, #9441, #7443, #8825, #3308, #6993, #8678, #5623, #7760, #1772, #6849, #1623, #1157 ), #4081 ) ;
#1934 = CYLINDRICAL_SURFACE ( 'NONE', #2171, 17.50000000000000355 ) ;
#1935 =( NAMED_UNIT ( * ) SI_UNIT ( $, .STERADIAN. ) SOLID_ANGLE_UNIT ( ) );
#1936 = ORIENTED_EDGE ( 'NONE', *, *, #6947, .T. ) ;
#1937 = AXIS2_PLACEMENT_3D ( 'NONE', #1537, #674, #2886 ) ;
#1938 = VERTEX_POINT ( 'NONE', #7280 ) ;
#1939 = DIRECTION ( 'NONE',  ( 1.069105884036591492E-50, -0.9997175446104182850, 0.02376617340079590149 ) ) ;
#1940 = VERTEX_POINT ( 'NONE', #2293 ) ;
#1941 = FACE_OUTER_BOUND ( 'NONE', #9328, .T. ) ;
#1942 = CARTESIAN_POINT ( 'NONE',  ( -12.37436867076458036, -12.37436867076458036, 19.62563132923542142 ) ) ;
#1943 = CARTESIAN_POINT ( 'NONE',  ( 53.29490495164537833, -48.67545040036924320, -60.28901569369803326 ) ) ;
#1944 = AXIS2_PLACEMENT_3D ( 'NONE', #7080, #6324, #8523 ) ;
#1945 = VECTOR ( 'NONE', #2086, 999.9999999999998863 ) ;
#1946 = CARTESIAN_POINT ( 'NONE',  ( 30.00000000000000000, 3.673940397442059178E-15, 2.999999999999999112 ) ) ;
#1947 = CYLINDRICAL_SURFACE ( 'NONE', #7408, 2.999999999999999112 ) ;
#1948 = ORIENTED_EDGE ( 'NONE', *, *, #4142, .T. ) ;
#1949 = EDGE_CURVE ( 'NONE', #3236, #3951, #4050, .T. ) ;
#1950 = ORIENTED_EDGE ( 'NONE', *, *, #7589, .T. ) ;
#1951 = CARTESIAN_POINT ( 'NONE',  ( -30.00000000000000000, 0.000000000000000000, 8.000000000000005329 ) ) ;
#1952 = AXIS2_PLACEMENT_3D ( 'NONE', #5784, #8084, #4437 ) ;
#1953 = ORIENTED_EDGE ( 'NONE', *, *, #3230, .T. ) ;
#1954 = ADVANCED_FACE ( 'NONE', ( #4313 ), #6621, .F. ) ;
#1955 = CIRCLE ( 'NONE', #2260, 3.000000000000000000 ) ;
#1956 = CARTESIAN_POINT ( 'NONE',  ( -4.119968255444916849E-15, -3.500000000000000000, 1.500000000000000000 ) ) ;
#1957 = EDGE_CURVE ( 'NONE', #6427, #8186, #1617, .T. ) ;
#1958 = DIRECTION ( 'NONE',  ( -1.000000000000000000, 0.000000000000000000, 0.000000000000000000 ) ) ;
#1959 = DIRECTION ( 'NONE',  ( -1.000000000000000000, -0.000000000000000000, -0.000000000000000000 ) ) ;
#1960 = AXIS2_PLACEMENT_3D ( 'NONE', #8220, #772, #730 ) ;
#1961 = EDGE_CURVE ( 'NONE', #2124, #6136, #5194, .T. ) ;
#1962 = DIRECTION ( 'NONE',  ( -1.000000000000000000, -0.000000000000000000, -0.000000000000000000 ) ) ;
#1963 = AXIS2_PLACEMENT_3D ( 'NONE', #2467, #9307, #1973 ) ;
#1964 = MECHANICAL_DESIGN_GEOMETRIC_PRESENTATION_REPRESENTATION (  '', ( #2424 ), #7788 ) ;
#1965 = CIRCLE ( 'NONE', #7475, 3.000000000000002665 ) ;
#1966 = DIRECTION ( 'NONE',  ( -1.000000000000000000, 0.000000000000000000, 0.000000000000000000 ) ) ;
#1967 = CARTESIAN_POINT ( 'NONE',  ( 27.74194578790375587, 4.529188556225775208, 1.101965149366711971 ) ) ;
#1968 = VECTOR ( 'NONE', #6001, 1000.000000000000000 ) ;
#1969 = VERTEX_POINT ( 'NONE', #5414 ) ;
#1970 = VERTEX_POINT ( 'NONE', #3921 ) ;
#1971 = CIRCLE ( 'NONE', #5964, 2.000000000000000000 ) ;
#1972 = CARTESIAN_POINT ( 'NONE',  ( 0.000000000000000000, 0.000000000000000000, 0.000000000000000000 ) ) ;
#1973 = DIRECTION ( 'NONE',  ( 0.000000000000000000, 0.000000000000000000, 1.000000000000000000 ) ) ;
#1974 = VERTEX_POINT ( 'NONE', #1668 ) ;
#1975 = VERTEX_POINT ( 'NONE', #8199 ) ;
#1976 = ORIENTED_EDGE ( 'NONE', *, *, #3015, .T. ) ;
#1977 = AXIS2_PLACEMENT_3D ( 'NONE', #786, #5841, #2952 ) ;
#1978 = EDGE_LOOP ( 'NONE', ( #4055, #1948, #716, #1144 ) ) ;
#1979 = CIRCLE ( 'NONE', #4894, 60.00000000000000000 ) ;
#1980 = FACE_OUTER_BOUND ( 'NONE', #8222, .T. ) ;
#1981 = APPLICATION_CONTEXT ( 'automotive_design' ) ;
#1982 = DIRECTION ( 'NONE',  ( -0.7071067811865444641, 0.7071067811865505703, -0.000000000000000000 ) ) ;
#1983 = CARTESIAN_POINT ( 'NONE',  ( -16.49999999999999645, -7.782354204448209592E-14, 5.000000000000000000 ) ) ;
#1984 = DIRECTION ( 'NONE',  ( 0.000000000000000000, 0.000000000000000000, 1.000000000000000000 ) ) ;
#1985 = CARTESIAN_POINT ( 'NONE',  ( 0.000000000000000000, 0.000000000000000000, 0.000000000000000000 ) ) ;
#1986 = VERTEX_POINT ( 'NONE', #4550 ) ;
#1987 = LINE ( 'NONE', #4911, #262 ) ;
#1988 = CARTESIAN_POINT ( 'NONE',  ( 43.21904109878573053, 80.45324141007795049, 43.95616229837705191 ) ) ;
#1989 = EDGE_LOOP ( 'NONE', ( #6194, #480, #5703, #4934, #7292, #8842, #7858, #5388, #2654, #6980, #6791, #7059, #8507, #1433 ) ) ;
#1990 = FACE_BOUND ( 'NONE', #9454, .T. ) ;
#1991 = CARTESIAN_POINT ( 'NONE',  ( -28.50000000000000000, -7.855833971761515132E-14, 1.500000000000037748 ) ) ;
#1992 =( BOUNDED_CURVE ( )  B_SPLINE_CURVE ( 3, ( #433, #6307, #6346, #4277 ),
 .UNSPECIFIED., .F., .T. ) 
 B_SPLINE_CURVE_WITH_KNOTS ( ( 4, 4 ),
 ( 2.356194490192344837, 3.141592653589793116 ),
 .UNSPECIFIED. ) 
 CURVE ( )  GEOMETRIC_REPRESENTATION_ITEM ( )  RATIONAL_B_SPLINE_CURVE ( ( 1.000000000000000000, 0.9492530216741911220, 0.9492530216741911220, 1.000000000000000000 ) ) 
 REPRESENTATION_ITEM ( '' )  );
#1993 = CARTESIAN_POINT ( 'NONE',  ( -7.180166011355011868, -26.02777777777776791, 0.000000000000000000 ) ) ;
#1994 = DIRECTION ( 'NONE',  ( 0.000000000000000000, 0.000000000000000000, -1.000000000000000000 ) ) ;
#1995 = DIRECTION ( 'NONE',  ( 0.000000000000000000, 0.000000000000000000, 1.000000000000000000 ) ) ;
#1996 = ORIENTED_EDGE ( 'NONE', *, *, #1912, .T. ) ;
#1997 = ORIENTED_EDGE ( 'NONE', *, *, #9457, .T. ) ;
#1998 = CARTESIAN_POINT ( 'NONE',  ( -0.7500000000000000000, 0.7500000000000000000, 1.500000000000000000 ) ) ;
#1999 = ORIENTED_EDGE ( 'NONE', *, *, #8529, .T. ) ;
#2000 = CARTESIAN_POINT ( 'NONE',  ( 0.000000000000000000, 0.000000000000000000, 0.000000000000000000 ) ) ;
#2001 = LINE ( 'NONE', #5889, #6430 ) ;
#2002 = DIRECTION ( 'NONE',  ( -1.000000000000000000, 0.000000000000000000, 0.000000000000000000 ) ) ;
#2003 = PLANE ( 'NONE',  #6616 ) ;
#2004 = EDGE_CURVE ( 'NONE', #8070, #6226, #5464, .T. ) ;
#2005 = CARTESIAN_POINT ( 'NONE',  ( -19.50000000000000355, 3.673940397442056417E-16, 10.00000000000000000 ) ) ;
#2006 = CIRCLE ( 'NONE', #9203, 8.000000000000017764 ) ;
#2007 = CARTESIAN_POINT ( 'NONE',  ( 5.000000000000000000, -14.14213562373112154, 14.14213562373418220 ) ) ;
#2008 = EDGE_CURVE ( 'NONE', #7855, #4159, #361, .T. ) ;
#2009 = ORIENTED_EDGE ( 'NONE', *, *, #7704, .T. ) ;
#2010 = ORIENTED_EDGE ( 'NONE', *, *, #829, .T. ) ;
#2011 = ADVANCED_FACE ( 'NONE', ( #986 ), #134, .F. ) ;
#2012 = ADVANCED_FACE ( 'NONE', ( #3826 ), #3063, .F. ) ;
#2013 = PRODUCT_DEFINITION_SHAPE ( 'NONE', 'NONE',  #9499 ) ;
#2014 = DIRECTION ( 'NONE',  ( 1.000000000000000000, 0.000000000000000000, 0.000000000000000000 ) ) ;
#2015 = DIRECTION ( 'NONE',  ( -1.000000000000000000, 0.000000000000000000, 0.000000000000000000 ) ) ;
#2016 = FACE_BOUND ( 'NONE', #2160, .T. ) ;
#2017 = CARTESIAN_POINT ( 'NONE',  ( 31.00000000000002132, 0.000000000000000000, 32.00000000000000000 ) ) ;
#2018 = VECTOR ( 'NONE', #2991, 1000.000000000000000 ) ;
#2019 = ORIENTED_EDGE ( 'NONE', *, *, #4534, .T. ) ;
#2020 = ORIENTED_EDGE ( 'NONE', *, *, #4070, .F. ) ;
#2021 = ORIENTED_EDGE ( 'NONE', *, *, #7626, .F. ) ;
#2022 = ORIENTED_EDGE ( 'NONE', *, *, #5730, .T. ) ;
#2023 = ADVANCED_FACE ( 'NONE', ( #1039 ), #843, .F. ) ;
#2024 = CARTESIAN_POINT ( 'NONE',  ( 32.00000000000000711, -34.99999999999999289, 58.99999999999997158 ) ) ;
#2025 = AXIS2_PLACEMENT_3D ( 'NONE', #7303, #61, #3752 ) ;
#2026 = CARTESIAN_POINT ( 'NONE',  ( 50.79490495164537833, -12.50000000000000000, -100.0000000000000000 ) ) ;
#2027 = FACE_OUTER_BOUND ( 'NONE', #5263, .T. ) ;
#2028 = ADVANCED_FACE ( 'NONE', ( #6190 ), #7424, .F. ) ;
#2029 = CARTESIAN_POINT ( 'NONE',  ( -26.42790562391193987, -6.696979066941380232, 0.2572250439434045632 ) ) ;
#2030 = FACE_BOUND ( 'NONE', #5175, .T. ) ;
#2031 = ORIENTED_EDGE ( 'NONE', *, *, #5155, .F. ) ;
#2032 = ORIENTED_EDGE ( 'NONE', *, *, #474, .T. ) ;
#2033 = DIRECTION ( 'NONE',  ( 0.000000000000000000, -0.9825825211874976706, 0.1858267716364374045 ) ) ;
#2034 = ORIENTED_EDGE ( 'NONE', *, *, #7580, .F. ) ;
#2035 = FACE_BOUND ( 'NONE', #4302, .T. ) ;
#2036 = AXIS2_PLACEMENT_3D ( 'NONE', #7883, #8558, #484 ) ;
#2037 = DIRECTION ( 'NONE',  ( 1.000000000000000000, 0.000000000000000000, -0.000000000000000000 ) ) ;
#2038 = FACE_OUTER_BOUND ( 'NONE', #1916, .T. ) ;
#2039 = CARTESIAN_POINT ( 'NONE',  ( -31.99999999999999289, 29.99999999999997868, 58.99999999999997158 ) ) ;
#2040 = DIRECTION ( 'NONE',  ( 0.000000000000000000, 0.000000000000000000, -1.000000000000000000 ) ) ;
#2041 = EDGE_LOOP ( 'NONE', ( #921, #321, #1193, #6734 ) ) ;
#2042 = VECTOR ( 'NONE', #2652, 1000.000000000000000 ) ;
#2043 = ORIENTED_EDGE ( 'NONE', *, *, #5760, .T. ) ;
#2044 = FACE_BOUND ( 'NONE', #9387, .T. ) ;
#2045 = ORIENTED_EDGE ( 'NONE', *, *, #6465, .T. ) ;
#2046 = EDGE_CURVE ( 'NONE', #7322, #4158, #6507, .T. ) ;
#2047 = CARTESIAN_POINT ( 'NONE',  ( 0.000000000000000000, 0.000000000000000000, 0.000000000000000000 ) ) ;
#2048 = DIRECTION ( 'NONE',  ( 0.7071067811865512365, 8.659560562354979697E-17, -0.7071067811865439090 ) ) ;
#2049 = AXIS2_PLACEMENT_3D ( 'NONE', #4606, #9064, #2496 ) ;
#2050 = LINE ( 'NONE', #1320, #7300 ) ;
#2051 = CARTESIAN_POINT ( 'NONE',  ( 62.09859669818811767, -30.00000000000000000, -66.51416582715444292 ) ) ;
#2052 = AXIS2_PLACEMENT_3D ( 'NONE', #6769, #8336, #3107 ) ;
#2053 = EDGE_CURVE ( 'NONE', #5050, #883, #4811, .T. ) ;
#2054 = CARTESIAN_POINT ( 'NONE',  ( 4.000000000000000000, -7.653668647303860872, -17.72759065022311731 ) ) ;
#2055 = DIRECTION ( 'NONE',  ( -1.000000000000000000, -0.000000000000000000, -0.000000000000000000 ) ) ;
#2056 = VERTEX_POINT ( 'NONE', #3978 ) ;
#2057 = ORIENTED_EDGE ( 'NONE', *, *, #5015, .T. ) ;
#2058 = FACE_OUTER_BOUND ( 'NONE', #151, .T. ) ;
#2059 = DIRECTION ( 'NONE',  ( -0.000000000000000000, -0.000000000000000000, -1.000000000000000000 ) ) ;
#2060 = CIRCLE ( 'NONE', #4512, 11.00000000000000711 ) ;
#2061 = VECTOR ( 'NONE', #6374, 1000.000000000000114 ) ;
#2062 = DIRECTION ( 'NONE',  ( 0.000000000000000000, 0.000000000000000000, 1.000000000000000000 ) ) ;
#2063 = CARTESIAN_POINT ( 'NONE',  ( 0.7500000000000000000, -0.7500000000000000000, 1.500000000000000000 ) ) ;
#2064 = ORIENTED_EDGE ( 'NONE', *, *, #5718, .T. ) ;
#2065 = ORIENTED_EDGE ( 'NONE', *, *, #3292, .T. ) ;
#2066 = ORIENTED_EDGE ( 'NONE', *, *, #1719, .F. ) ;
#2067 = ORIENTED_EDGE ( 'NONE', *, *, #4257, .F. ) ;
#2068 = EDGE_CURVE ( 'NONE', #3926, #5660, #7414, .T. ) ;
#2069 = DIRECTION ( 'NONE',  ( 0.000000000000000000, 0.000000000000000000, 1.000000000000000000 ) ) ;
#2070 = AXIS2_PLACEMENT_3D ( 'NONE', #1638, #8979, #204 ) ;
#2071 = CARTESIAN_POINT ( 'NONE',  ( 0.7500000000000000000, 0.7500000000000000000, 1.500000000000000000 ) ) ;
#2072 = AXIS2_PLACEMENT_3D ( 'NONE', #2614, #5545, #8470 ) ;
#2073 = CARTESIAN_POINT ( 'NONE',  ( 60.00000000000000000, -15.90990257669733943, -54.09009742330271564 ) ) ;
#2074 = DIRECTION ( 'NONE',  ( -0.000000000000000000, -0.000000000000000000, 1.000000000000000000 ) ) ;
#2075 = CARTESIAN_POINT ( 'NONE',  ( -0.7500000000000000000, 0.7500000000000000000, 1.500000000000000000 ) ) ;
#2076 = ORIENTED_EDGE ( 'NONE', *, *, #8303, .T. ) ;
#2077 = CARTESIAN_POINT ( 'NONE',  ( 60.00000000000000000, -15.90990257669733943, -82.90990257669729147 ) ) ;
#2078 = ORIENTED_EDGE ( 'NONE', *, *, #6483, .F. ) ;
#2079 = AXIS2_PLACEMENT_3D ( 'NONE', #6281, #719, #2668 ) ;
#2080 = CARTESIAN_POINT ( 'NONE',  ( -28.32042821893188744, 1.471975546721317141, 1.357900206176153146 ) ) ;
#2081 = CARTESIAN_POINT ( 'NONE',  ( 26.21170834203226718, -53.97171801779368394, -2.612255525622730001 ) ) ;
#2082 = PLANE ( 'NONE',  #5291 ) ;
#2083 = CARTESIAN_POINT ( 'NONE',  ( 2.819222834329444538, -27.81181297095828597, 0.9517275379012076764 ) ) ;
#2084 = ORIENTED_EDGE ( 'NONE', *, *, #9254, .F. ) ;
#2085 = EDGE_LOOP ( 'NONE', ( #2839, #8017, #2157, #2479 ) ) ;
#2086 = DIRECTION ( 'NONE',  ( 0.000000000000000000, -0.7071067811865479058, 0.7071067811865472397 ) ) ;
#2087 = ORIENTED_EDGE ( 'NONE', *, *, #3950, .T. ) ;
#2088 = CYLINDRICAL_SURFACE ( 'NONE', #3504, 17.50000000000000355 ) ;
#2089 = FACE_OUTER_BOUND ( 'NONE', #7476, .T. ) ;
#2090 = DIRECTION ( 'NONE',  ( 1.000000000000000000, 0.000000000000000000, 0.000000000000000000 ) ) ;
#2091 = AXIS2_PLACEMENT_3D ( 'NONE', #6944, #4060, #9138 ) ;
#2092 = AXIS2_PLACEMENT_3D ( 'NONE', #232, #9061, #4746 ) ;
#2093 = FACE_BOUND ( 'NONE', #3877, .T. ) ;
#2094 = CARTESIAN_POINT ( 'NONE',  ( 4.000000000000000888, 2.143131898507868248E-15, -17.50000000000000000 ) ) ;
#2095 = LINE ( 'NONE', #3008, #428 ) ;
#2096 = VECTOR ( 'NONE', #1347, 1000.000000000000000 ) ;
#2097 = EDGE_LOOP ( 'NONE', ( #9390, #425, #6461, #3010 ) ) ;
#2098 = ORIENTED_EDGE ( 'NONE', *, *, #4434, .F. ) ;
#2099 = VECTOR ( 'NONE', #7500, 1000.000000000000000 ) ;
#2100 = DIRECTION ( 'NONE',  ( 1.000000000000000000, 0.000000000000000000, 0.000000000000000000 ) ) ;
#2101 = EDGE_CURVE ( 'NONE', #2895, #8186, #9099, .T. ) ;
#2102 = AXIS2_PLACEMENT_3D ( 'NONE', #7684, #9113, #6057 ) ;
#2103 = VECTOR ( 'NONE', #6487, 1000.000000000000000 ) ;
#2104 = CARTESIAN_POINT ( 'NONE',  ( 60.00000000000000000, 15.90990257669733943, -88.90990257669730568 ) ) ;
#2105 = VECTOR ( 'NONE', #6829, 1000.000000000000000 ) ;
#2106 = AXIS2_PLACEMENT_3D ( 'NONE', #4794, #3302, #1865 ) ;
#2107 = DIRECTION ( 'NONE',  ( -0.000000000000000000, -0.000000000000000000, -1.000000000000000000 ) ) ;
#2108 = CYLINDRICAL_SURFACE ( 'NONE', #5022, 0.7500000000012114754 ) ;
#2109 = VECTOR ( 'NONE', #5620, 1000.000000000000000 ) ;
#2110 = ORIENTED_EDGE ( 'NONE', *, *, #4596, .F. ) ;
#2111 = ORIENTED_EDGE ( 'NONE', *, *, #135, .F. ) ;
#2112 = ADVANCED_FACE ( 'NONE', ( #4646 ), #7570, .F. ) ;
#2113 = VERTEX_POINT ( 'NONE', #9337 ) ;
#2114 = CIRCLE ( 'NONE', #6277, 0.7500000000001915135 ) ;
#2115 = EDGE_LOOP ( 'NONE', ( #2547, #6798, #831, #4788, #4948, #397 ) ) ;
#2116 = CARTESIAN_POINT ( 'NONE',  ( 28.50000000000000355, 2.364097784513999692E-13, 5.000000000000000000 ) ) ;
#2117 = AXIS2_PLACEMENT_3D ( 'NONE', #4837, #7817, #2818 ) ;
#2118 = DIRECTION ( 'NONE',  ( -1.000000000000000000, 0.000000000000000000, 0.000000000000000000 ) ) ;
#2119 = CARTESIAN_POINT ( 'NONE',  ( -31.99999999999999289, 0.000000000000000000, 50.50000000000001421 ) ) ;
#2120 = DIRECTION ( 'NONE',  ( -1.000000000000000000, -0.000000000000000000, -0.000000000000000000 ) ) ;
#2121 = EDGE_CURVE ( 'NONE', #4182, #5535, #7809, .T. ) ;
#2122 = PLANE ( 'NONE',  #9006 ) ;
#2123 = VECTOR ( 'NONE', #4164, 1000.000000000000000 ) ;
#2124 = VERTEX_POINT ( 'NONE', #7672 ) ;
#2125 = EDGE_CURVE ( 'NONE', #18, #2310, #5513, .T. ) ;
#2126 = DIRECTION ( 'NONE',  ( 0.000000000000000000, 0.7071067811865479058, -0.7071067811865472397 ) ) ;
#2127 = EDGE_CURVE ( 'NONE', #2772, #6441, #2770, .T. ) ;
#2128 = ADVANCED_FACE ( 'NONE', ( #4157 ), #5280, .F. ) ;
#2129 = ORIENTED_EDGE ( 'NONE', *, *, #535, .F. ) ;
#2130 = CARTESIAN_POINT ( 'NONE',  ( 16.00000000000000000, 21.00000000000000000, -16.89999999999999858 ) ) ;
#2131 = DIRECTION ( 'NONE',  ( 0.000000000000000000, 0.000000000000000000, 1.000000000000000000 ) ) ;
#2132 = AXIS2_PLACEMENT_3D ( 'NONE', #62, #8132, #8840 ) ;
#2133 = CARTESIAN_POINT ( 'NONE',  ( 22.50000000000000355, 2.356749903719115078E-13, 5.000000000000000000 ) ) ;
#2134 = DIRECTION ( 'NONE',  ( -1.000000000000000000, -0.000000000000000000, -0.000000000000000000 ) ) ;
#2135 = DIRECTION ( 'NONE',  ( -1.000000000000000000, 0.000000000000000000, 0.000000000000000000 ) ) ;
#2136 = ORIENTED_EDGE ( 'NONE', *, *, #1836, .T. ) ;
#2137 = EDGE_CURVE ( 'NONE', #6770, #2908, #6423, .T. ) ;
#2138 = EDGE_LOOP ( 'NONE', ( #8490, #1891, #2158, #2010 ) ) ;
#2139 = ORIENTED_EDGE ( 'NONE', *, *, #9357, .T. ) ;
#2140 = ADVANCED_FACE ( 'NONE', ( #9239 ), #2582, .F. ) ;
#2141 = CARTESIAN_POINT ( 'NONE',  ( -28.27439555746436284, -1.684082973785163029, 1.321420441384538069 ) ) ;
#2142 = DIRECTION ( 'NONE',  ( 9.614813431917774709E-17, 0.7071067811865493491, -0.7071067811865455743 ) ) ;
#2143 = EDGE_CURVE ( 'NONE', #7322, #4945, #7084, .T. ) ;
#2144 = CARTESIAN_POINT ( 'NONE',  ( 27.00000000000000000, 43.00000000000000000, -25.00000000000000000 ) ) ;
#2145 = LINE ( 'NONE', #2051, #2478 ) ;
#2146 = CARTESIAN_POINT ( 'NONE',  ( -53.29490495164537833, -15.90990257669733943, -57.09009742330271564 ) ) ;
#2147 = FACE_OUTER_BOUND ( 'NONE', #4203, .T. ) ;
#2148 = EDGE_LOOP ( 'NONE', ( #3204, #7272, #8999, #324, #1275, #1176 ) ) ;
#2149 = EDGE_LOOP ( 'NONE', ( #5067, #8555, #846, #1075 ) ) ;
#2150 = DIRECTION ( 'NONE',  ( -1.000000000000000000, -0.000000000000000000, -0.000000000000000000 ) ) ;
#2151 = ITEM_DEFINED_TRANSFORMATION ( 'NONE', 'NONE', #5623,  #1614 ) ;
#2152 = DIRECTION ( 'NONE',  ( 0.000000000000000000, 1.000000000000000000, 0.000000000000000000 ) ) ;
#2153 = VECTOR ( 'NONE', #6479, 1000.000000000000000 ) ;
#2154 = FACE_BOUND ( 'NONE', #8202, .T. ) ;
#2155 =( REPRESENTATION_RELATIONSHIP ('NONE','NONE', #1933, #8501 ) REPRESENTATION_RELATIONSHIP_WITH_TRANSFORMATION ( #5721 )SHAPE_REPRESENTATION_RELATIONSHIP( ) );
#2156 = CARTESIAN_POINT ( 'NONE',  ( -37.00000000000000711, -3.673940397442057600E-15, -55.00000000000000711 ) ) ;
#2157 = ORIENTED_EDGE ( 'NONE', *, *, #3307, .F. ) ;
#2158 = ORIENTED_EDGE ( 'NONE', *, *, #9316, .T. ) ;
#2159 = VERTEX_POINT ( 'NONE', #5654 ) ;
#2160 = EDGE_LOOP ( 'NONE', ( #5099, #2087 ) ) ;
#2161 = ADVANCED_FACE ( 'NONE', ( #4021 ), #4876, .F. ) ;
#2162 = CARTESIAN_POINT ( 'NONE',  ( 28.45342843414351464, -0.8561988828940789720, 1.463295953604768940 ) ) ;
#2163 = CARTESIAN_POINT ( 'NONE',  ( 7.180166011355011868, -26.02777777777776436, 0.000000000000000000 ) ) ;
#2164 = DIRECTION ( 'NONE',  ( 0.000000000000000000, 0.000000000000000000, -1.000000000000000000 ) ) ;
#2165 = DIRECTION ( 'NONE',  ( 0.7071067811865469066, 8.659560562354925463E-17, -0.7071067811865481278 ) ) ;
#2166 = LINE ( 'NONE', #5295, #6591 ) ;
#2167 = FACE_BOUND ( 'NONE', #1497, .T. ) ;
#2168 = ORIENTED_EDGE ( 'NONE', *, *, #5155, .T. ) ;
#2169 = LINE ( 'NONE', #636, #5333 ) ;
#2170 = ORIENTED_EDGE ( 'NONE', *, *, #8695, .F. ) ;
#2171 = AXIS2_PLACEMENT_3D ( 'NONE', #2891, #2074, #7796 ) ;
#2172 = CARTESIAN_POINT ( 'NONE',  ( 12.37436867076458036, -12.37436867076458036, 19.62563132923542142 ) ) ;
#2173 = FACE_BOUND ( 'NONE', #2669, .T. ) ;
#2174 = LINE ( 'NONE', #7313, #2454 ) ;
#2175 = ADVANCED_FACE ( 'NONE', ( #4921 ), #6994, .T. ) ;
#2176 = CARTESIAN_POINT ( 'NONE',  ( 0.000000000000000000, 0.000000000000000000, 27.50000000000000355 ) ) ;
#2177 = EDGE_CURVE ( 'NONE', #1699, #4010, #3290, .T. ) ;
#2178 = ORIENTED_EDGE ( 'NONE', *, *, #4216, .T. ) ;
#2179 = EDGE_LOOP ( 'NONE', ( #4949, #30, #4923, #6668 ) ) ;
#2180 = SURFACE_STYLE_FILL_AREA ( #6565 ) ;
#2181 = VECTOR ( 'NONE', #347, 1000.000000000000000 ) ;
#2182 = ORIENTED_EDGE ( 'NONE', *, *, #594, .F. ) ;
#2183 = DIRECTION ( 'NONE',  ( -1.000000000000000000, 0.000000000000000000, 0.000000000000000000 ) ) ;
#2184 = CYLINDRICAL_SURFACE ( 'NONE', #289, 15.00000000000000000 ) ;
#2185 = B_SPLINE_CURVE_WITH_KNOTS ( 'NONE', 3,
 ( #3523, #4576, #7996, #5249, #2083, #689, #4345, #2859, #5748, #920, #6020, #1407, #5297, #2811, #3852, #9385, #8176, #5791, #7952, #6788, #6562, #1364 ),
 .UNSPECIFIED., .F., .F.,
 ( 4, 2, 2, 2, 2, 2, 2, 2, 2, 2, 4 ),
 ( 1.026960276838673439E-18, 0.001276335940410830774, 0.002552671880821660248, 0.003829007821232489721, 0.004467175791437904241, 0.005105343761643319628, 0.006381679702054149535, 0.007019847672259564055, 0.007658015642464980309, 0.008934351582875806747, 0.01021068752328663232 ),
 .UNSPECIFIED. ) ;
#2186 = EDGE_CURVE ( 'NONE', #4100, #6191, #5884, .T. ) ;
#2187 = DIRECTION ( 'NONE',  ( 0.000000000000000000, 0.7071067811865477948, -0.7071067811865473507 ) ) ;
#2188 = LINE ( 'NONE', #655, #2153 ) ;
#2190 = CYLINDRICAL_SURFACE ( 'NONE', #8204, 2.999999999999999112 ) ;
#2189 = CIRCLE ( 'NONE', #3415, 30.00000000000000000 ) ;
#2191 = EDGE_CURVE ( 'NONE', #5210, #4201, #4664, .T. ) ;
#2192 = CARTESIAN_POINT ( 'NONE',  ( 0.000000000000000000, 34.00000000000001421, 32.00000000000000000 ) ) ;
#2193 = DIRECTION ( 'NONE',  ( 1.000000000000000000, 0.000000000000000000, 0.000000000000000000 ) ) ;
#2194 = ORIENTED_EDGE ( 'NONE', *, *, #2923, .T. ) ;
#2195 = VERTEX_POINT ( 'NONE', #6288 ) ;
#2196 = DIRECTION ( 'NONE',  ( 0.000000000000000000, -0.7071067811865479058, 0.7071067811865472397 ) ) ;
#2197 = FACE_OUTER_BOUND ( 'NONE', #5985, .T. ) ;
#2198 = VECTOR ( 'NONE', #2107, 1000.000000000000000 ) ;
#2199 = DIRECTION ( 'NONE',  ( -1.000000000000000000, 0.000000000000000000, 0.000000000000000000 ) ) ;
#2200 = PLANE ( 'NONE',  #1907 ) ;
#2201 = LINE ( 'NONE', #3074, #9300 ) ;
#2202 = EDGE_LOOP ( 'NONE', ( #3842, #5725, #948, #3193 ) ) ;
#2203 = ORIENTED_EDGE ( 'NONE', *, *, #2322, .F. ) ;
#2204 = ORIENTED_EDGE ( 'NONE', *, *, #5774, .T. ) ;
#2205 = CARTESIAN_POINT ( 'NONE',  ( -56.07586385285962649, 96.36314398677498616, 59.86606487507404495 ) ) ;
#2206 = ORIENTED_EDGE ( 'NONE', *, *, #9101, .T. ) ;
#2207 = AXIS2_PLACEMENT_3D ( 'NONE', #6872, #374, #332 ) ;
#2208 = FACE_OUTER_BOUND ( 'NONE', #8058, .T. ) ;
#2209 = DIRECTION ( 'NONE',  ( 0.000000000000000000, 1.000000000000000000, 0.000000000000000000 ) ) ;
#2210 = CIRCLE ( 'NONE', #1441, 11.00000000000000711 ) ;
#2211 = CARTESIAN_POINT ( 'NONE',  ( 4.000000000000000000, 14.14213562373247868, 14.14213562373282329 ) ) ;
#2212 = DIRECTION ( 'NONE',  ( -1.000000000000000000, -0.000000000000000000, -0.000000000000000000 ) ) ;
#2213 = PLANE ( 'NONE',  #2601 ) ;
#2214 = EDGE_CURVE ( 'NONE', #2638, #9368, #1128, .T. ) ;
#2215 = CARTESIAN_POINT ( 'NONE',  ( -22.50000000000000355, 0.000000000000000000, 10.00000000000000000 ) ) ;
#2216 = ORIENTED_EDGE ( 'NONE', *, *, #3051, .F. ) ;
#2217 = FACE_OUTER_BOUND ( 'NONE', #3708, .T. ) ;
#2218 = CIRCLE ( 'NONE', #2070, 0.7500000000012114754 ) ;
#2219 = ORIENTED_EDGE ( 'NONE', *, *, #6195, .F. ) ;
#2220 = EDGE_CURVE ( 'NONE', #106, #6587, #6199, .T. ) ;
#2221 = FACE_OUTER_BOUND ( 'NONE', #9411, .T. ) ;
#2222 = CARTESIAN_POINT ( 'NONE',  ( 3.499999999999999556, 0.000000000000000000, 0.000000000000000000 ) ) ;
#2223 = DIRECTION ( 'NONE',  ( 0.000000000000000000, 0.000000000000000000, 1.000000000000000000 ) ) ;
#2224 = EDGE_LOOP ( 'NONE', ( #2611, #8669 ) ) ;
#2225 = AXIS2_PLACEMENT_3D ( 'NONE', #4102, #3421, #6410 ) ;
#2226 = EDGE_LOOP ( 'NONE', ( #2710, #3476, #9215, #7680 ) ) ;
#2227 = ORIENTED_EDGE ( 'NONE', *, *, #6711, .T. ) ;
#2228 = CARTESIAN_POINT ( 'NONE',  ( -51.96152422706632024, -30.00000000000000000, -13.00000000000000000 ) ) ;
#2229 = DIRECTION ( 'NONE',  ( 0.7071067811865435759, 0.000000000000000000, 0.7071067811865513475 ) ) ;
#2230 = CARTESIAN_POINT ( 'NONE',  ( 0.000000000000000000, 18.47759065022658120, 7.653668647302884764 ) ) ;
#2231 = DIRECTION ( 'NONE',  ( 0.000000000000000000, 0.000000000000000000, 1.000000000000000000 ) ) ;
#2232 = AXIS2_PLACEMENT_3D ( 'NONE', #4569, #6114, #1634 ) ;
#2233 = CARTESIAN_POINT ( 'NONE',  ( 60.00000000000000000, -30.00000000000000000, -30.00000000000000000 ) ) ;
#2234 = EDGE_CURVE ( 'NONE', #2537, #2895, #7128, .T. ) ;
#2235 = DIRECTION ( 'NONE',  ( -0.000000000000000000, -0.000000000000000000, -1.000000000000000000 ) ) ;
#2236 = LINE ( 'NONE', #8054, #5497 ) ;
#2237 = ADVANCED_FACE ( 'NONE', ( #8531 ), #1947, .F. ) ;
#2238 = ORIENTED_EDGE ( 'NONE', *, *, #731, .F. ) ;
#2239 = ADVANCED_FACE ( 'NONE', ( #3083 ), #3132, .F. ) ;
#2240 = EDGE_LOOP ( 'NONE', ( #7413, #1997 ) ) ;
#2241 = AXIS2_PLACEMENT_3D ( 'NONE', #1166, #496, #2037 ) ;
#2242 = DIRECTION ( 'NONE',  ( 0.000000000000000000, 0.000000000000000000, 1.000000000000000000 ) ) ;
#2243 = DIRECTION ( 'NONE',  ( -1.000000000000000000, 0.000000000000000000, 0.000000000000000000 ) ) ;
#2244 = ADVANCED_FACE ( 'NONE', ( #6746 ), #163, .F. ) ;
#2245 = EDGE_LOOP ( 'NONE', ( #8109, #4946, #9230, #505 ) ) ;
#2246 = PRODUCT_DEFINITION_SHAPE ( 'NONE', 'NONE',  #9489 ) ;
#2247 = CARTESIAN_POINT ( 'NONE',  ( -3.614752790974351981, 28.10687131109265735, 1.336560128559570959 ) ) ;
#2248 = CIRCLE ( 'NONE', #7622, 0.7500000000017874591 ) ;
#2249 = EDGE_CURVE ( 'NONE', #8566, #9251, #5109, .T. ) ;
#2250 = DIRECTION ( 'NONE',  ( -1.000000000000000000, -0.000000000000000000, -0.000000000000000000 ) ) ;
#2251 = DIRECTION ( 'NONE',  ( -1.000000000000000000, 0.000000000000000000, -0.000000000000000000 ) ) ;
#2252 = ORIENTED_EDGE ( 'NONE', *, *, #5423, .T. ) ;
#2253 = ORIENTED_EDGE ( 'NONE', *, *, #8813, .T. ) ;
#2254 = CIRCLE ( 'NONE', #4867, 18.50000000000001776 ) ;
#2255 = EDGE_CURVE ( 'NONE', #3092, #7550, #9405, .T. ) ;
#2256 = DIRECTION ( 'NONE',  ( -1.085978143626196945E-16, -0.9911323735125173728, 0.1328782080532535659 ) ) ;
#2257 = CIRCLE ( 'NONE', #5026, 3.000000000000000000 ) ;
#2258 = ORIENTED_EDGE ( 'NONE', *, *, #5662, .F. ) ;
#2259 = EDGE_CURVE ( 'NONE', #8340, #580, #7221, .T. ) ;
#2260 = AXIS2_PLACEMENT_3D ( 'NONE', #4342, #8946, #7312 ) ;
#2261 = PLANE ( 'NONE',  #1937 ) ;
#2262 = EDGE_CURVE ( 'NONE', #2573, #4625, #2516, .T. ) ;
#2263 = DIRECTION ( 'NONE',  ( -1.000000000000000000, 0.000000000000000000, 0.000000000000000000 ) ) ;
#2264 = AXIS2_PLACEMENT_3D ( 'NONE', #7211, #4379, #6361 ) ;
#2265 = CARTESIAN_POINT ( 'NONE',  ( 0.7500000000000000000, 0.7500000000000000000, 0.000000000000000000 ) ) ;
#2266 = AXIS2_PLACEMENT_3D ( 'NONE', #5172, #8870, #2193 ) ;
#2267 = DIRECTION ( 'NONE',  ( 0.000000000000000000, 0.000000000000000000, -1.000000000000000000 ) ) ;
#2268 = DIRECTION ( 'NONE',  ( -0.000000000000000000, -0.000000000000000000, -1.000000000000000000 ) ) ;
#2269 = CIRCLE ( 'NONE', #7790, 3.000000000000002665 ) ;
#2270 = CARTESIAN_POINT ( 'NONE',  ( -26.21170834203230982, 53.97171801779368394, -0.5000000000000038858 ) ) ;
#2271 = ORIENTED_EDGE ( 'NONE', *, *, #3994, .F. ) ;
#2272 = CARTESIAN_POINT ( 'NONE',  ( 5.000000000000000000, 18.47759065022580316, -7.653668647301631545 ) ) ;
#2273 = ORIENTED_EDGE ( 'NONE', *, *, #1925, .T. ) ;
#2274 = DIRECTION ( 'NONE',  ( 1.000000000000000000, 0.000000000000000000, 0.000000000000000000 ) ) ;
#2275 = DIRECTION ( 'NONE',  ( 0.000000000000000000, -0.000000000000000000, 1.000000000000000000 ) ) ;
#2276 = LINE ( 'NONE', #6029, #6897 ) ;
#2277 = CIRCLE ( 'NONE', #9324, 7.250000000000002665 ) ;
#2278 = CARTESIAN_POINT ( 'NONE',  ( 60.00000000000000000, -3.673940397442057600E-15, -70.00000000000000000 ) ) ;
#2279 = AXIS2_PLACEMENT_3D ( 'NONE', #3372, #6355, #1298 ) ;
#2280 = VERTEX_POINT ( 'NONE', #2370 ) ;
#2281 = ORIENTED_EDGE ( 'NONE', *, *, #7530, .F. ) ;
#2282 = EDGE_LOOP ( 'NONE', ( #8804, #7900, #4058, #5658, #9326, #1264 ) ) ;
#2283 = ORIENTED_EDGE ( 'NONE', *, *, #1719, .T. ) ;
#2284 = CARTESIAN_POINT ( 'NONE',  ( 4.000000000000000000, -7.653668647301985040, 18.47759065022880520 ) ) ;
#2285 = CYLINDRICAL_SURFACE ( 'NONE', #8111, 6.000000000000000000 ) ;
#2286 = VECTOR ( 'NONE', #3724, 1000.000000000000000 ) ;
#2287 = DIRECTION ( 'NONE',  ( -0.000000000000000000, -0.000000000000000000, 1.000000000000000000 ) ) ;
#2288 = AXIS2_PLACEMENT_3D ( 'NONE', #1841, #1697, #5498 ) ;
#2289 =( REPRESENTATION_RELATIONSHIP ('NONE','NONE', #1933, #7573 ) REPRESENTATION_RELATIONSHIP_WITH_TRANSFORMATION ( #1003 )SHAPE_REPRESENTATION_RELATIONSHIP( ) );
#2290 = CARTESIAN_POINT ( 'NONE',  ( 0.000000000000000000, 0.000000000000000000, 11.00000000000000000 ) ) ;
#2291 = CARTESIAN_POINT ( 'NONE',  ( 25.50000000000000355, 3.673940397442054445E-16, 5.000000000000000000 ) ) ;
#2292 = CARTESIAN_POINT ( 'NONE',  ( -12.37436867076458036, -12.37436867076458036, 44.37436867076458213 ) ) ;
#2293 = CARTESIAN_POINT ( 'NONE',  ( -3.000000000000000000, -22.50000000000000355, 10.00000000000000000 ) ) ;
#2294 = VERTEX_POINT ( 'NONE', #600 ) ;
#2295 = ORIENTED_EDGE ( 'NONE', *, *, #3626, .T. ) ;
#2296 = CARTESIAN_POINT ( 'NONE',  ( 4.000000000000000000, 18.47759065022658120, 6.903668647304224137 ) ) ;
#2297 = CARTESIAN_POINT ( 'NONE',  ( -3.500000000000000000, 4.119968255444916849E-15, 1.500000000000000000 ) ) ;
#2298 = ORIENTED_EDGE ( 'NONE', *, *, #7347, .F. ) ;
#2299 = LINE ( 'NONE', #3785, #1191 ) ;
#2300 = EDGE_CURVE ( 'NONE', #6171, #106, #2185, .T. ) ;
#2301 = CIRCLE ( 'NONE', #5989, 3.000000000000002665 ) ;
#2302 =( BOUNDED_CURVE ( )  B_SPLINE_CURVE ( 3, ( #8197, #1613, #3104, #5993 ),
 .UNSPECIFIED., .F., .F. ) 
 B_SPLINE_CURVE_WITH_KNOTS ( ( 4, 4 ),
 ( 5.497787143782137953, 7.068583470577034511 ),
 .UNSPECIFIED. ) 
 CURVE ( )  GEOMETRIC_REPRESENTATION_ITEM ( )  RATIONAL_B_SPLINE_CURVE ( ( 1.000000000000000000, 0.8047378541243649375, 0.8047378541243649375, 1.000000000000000000 ) ) 
 REPRESENTATION_ITEM ( '' )  );
#2303 = EDGE_CURVE ( 'NONE', #7086, #4536, #214, .T. ) ;
#2304 = DIRECTION ( 'NONE',  ( 0.000000000000000000, 0.000000000000000000, -1.000000000000000000 ) ) ;
#2305 = ADVANCED_FACE ( 'NONE', ( #3572 ), #5144, .F. ) ;
#2306 = EDGE_CURVE ( 'NONE', #7179, #6408, #8941, .T. ) ;
#2307 = PRODUCT_DEFINITION_CONTEXT ( 'detailed design', #1295, 'design' ) ;
#2308 = PLANE ( 'NONE',  #876 ) ;
#2309 = EDGE_LOOP ( 'NONE', ( #2034, #7755, #8579, #1130 ) ) ;
#2310 = VERTEX_POINT ( 'NONE', #4521 ) ;
#2311 = CARTESIAN_POINT ( 'NONE',  ( -56.07586385285965491, 64.54333883338061639, 28.04625972167975334 ) ) ;
#2312 = FACE_OUTER_BOUND ( 'NONE', #4683, .T. ) ;
#2313 = AXIS2_PLACEMENT_3D ( 'NONE', #9293, #8585, #4264 ) ;
#2314 = DIRECTION ( 'NONE',  ( -0.000000000000000000, -0.000000000000000000, 1.000000000000000000 ) ) ;
#2315 = EDGE_CURVE ( 'NONE', #703, #4100, #7448, .T. ) ;
#2316 = CARTESIAN_POINT ( 'NONE',  ( 6.000000000000000888, -22.50000000000000355, 5.000000000000000000 ) ) ;
#2317 = DIRECTION ( 'NONE',  ( 0.000000000000000000, 0.000000000000000000, -1.000000000000000000 ) ) ;
#2318 = FACE_OUTER_BOUND ( 'NONE', #6956, .T. ) ;
#2319 = CARTESIAN_POINT ( 'NONE',  ( 60.00000000000000000, 15.90990257669733943, -88.90990257669730568 ) ) ;
#2320 = DIRECTION ( 'NONE',  ( -0.7071067811865435759, 8.659560562354886020E-17, 0.7071067811865513475 ) ) ;
#2321 = CIRCLE ( 'NONE', #6003, 17.50000000000000000 ) ;
#2322 = EDGE_CURVE ( 'NONE', #4035, #3697, #3803, .T. ) ;
#2323 = VERTEX_POINT ( 'NONE', #4720 ) ;
#2324 = SURFACE_SIDE_STYLE ('',( #3855 ) ) ;
#2325 = EDGE_LOOP ( 'NONE', ( #6236, #692, #563, #2031 ) ) ;
#2326 = CARTESIAN_POINT ( 'NONE',  ( 0.000000000000000000, 0.000000000000000000, 0.000000000000000000 ) ) ;
#2327 = CARTESIAN_POINT ( 'NONE',  ( 5.000000000000000000, 7.653668647302530381, 18.47759065022802716 ) ) ;
#2328 = EDGE_CURVE ( 'NONE', #4422, #5465, #9248, .T. ) ;
#2329 = DIRECTION ( 'NONE',  ( 1.000000000000000000, 0.000000000000000000, 0.000000000000000000 ) ) ;
#2330 = CARTESIAN_POINT ( 'NONE',  ( 60.00000000000000000, -15.90990257669733943, -54.09009742330271564 ) ) ;
#2331 = VERTEX_POINT ( 'NONE', #4621 ) ;
#2332 = VECTOR ( 'NONE', #6653, 1000.000000000000114 ) ;
#2333 = PRODUCT_DEFINITION_SHAPE ( 'NONE', 'NONE',  #9480 ) ;
#2334 = VERTEX_POINT ( 'NONE', #4766 ) ;
#2335 = ORIENTED_EDGE ( 'NONE', *, *, #3834, .F. ) ;
#2336 = DIRECTION ( 'NONE',  ( 0.000000000000000000, 0.000000000000000000, -1.000000000000000000 ) ) ;
#2337 = EDGE_LOOP ( 'NONE', ( #6995, #4484, #4817, #4224, #6540 ) ) ;
#2338 = CARTESIAN_POINT ( 'NONE',  ( 0.000000000000000000, 0.000000000000000000, 5.000000000000000000 ) ) ;
#2339 = CARTESIAN_POINT ( 'NONE',  ( 0.000000000000000000, 0.000000000000000000, 10.00000000000000000 ) ) ;
#2340 = DIRECTION ( 'NONE',  ( 1.000000000000000000, -0.000000000000000000, -0.000000000000000000 ) ) ;
#2341=STYLED_ITEM('',(#9515),#6309);
#2342 = CARTESIAN_POINT ( 'NONE',  ( 60.00000000000000000, 15.90990257669733943, -54.09009742330271564 ) ) ;
#2343 = DIRECTION ( 'NONE',  ( 0.000000000000000000, 0.000000000000000000, -1.000000000000000000 ) ) ;
#2344 = CARTESIAN_POINT ( 'NONE',  ( 27.00000000000000000, 43.00000000000000000, 11.99999999999999645 ) ) ;
#2345 = VECTOR ( 'NONE', #4771, 1000.000000000000114 ) ;
#2346 = CARTESIAN_POINT ( 'NONE',  ( 28.21952111405551022, -3.291689805591845541, 1.408977859035689617 ) ) ;
#2347 = EDGE_CURVE ( 'NONE', #4182, #1107, #2813, .T. ) ;
#2348 = VERTEX_POINT ( 'NONE', #2468 ) ;
#2349 = ORIENTED_EDGE ( 'NONE', *, *, #932, .F. ) ;
#2350 = DIRECTION ( 'NONE',  ( 1.000000000000000000, 0.000000000000000000, 0.000000000000000000 ) ) ;
#2351 = ORIENTED_EDGE ( 'NONE', *, *, #2550, .F. ) ;
#2352 = ADVANCED_FACE ( 'NONE', ( #7740 ), #4806, .F. ) ;
#2353 = CIRCLE ( 'NONE', #7250, 15.00000000000000000 ) ;
#2354 = CARTESIAN_POINT ( 'NONE',  ( -3.299340129088522922, 28.21697752735853726, 1.407342696159064488 ) ) ;
#2355 = FACE_BOUND ( 'NONE', #6160, .T. ) ;
#2356 = DIRECTION ( 'NONE',  ( 0.5773502691896290617, -0.5773502691896258421, 0.5773502691896225114 ) ) ;
#2357 = EDGE_LOOP ( 'NONE', ( #7252, #1618, #8178, #33 ) ) ;
#2358 = ORIENTED_EDGE ( 'NONE', *, *, #3869, .T. ) ;
#2359 = VECTOR ( 'NONE', #9212, 1000.000000000000000 ) ;
#2360 = APPLICATION_PROTOCOL_DEFINITION ( 'draft international standard', 'automotive_design', 1998, #1295 ) ;
#2361 = LINE ( 'NONE', #2409, #5318 ) ;
#2362 =( BOUNDED_CURVE ( )  B_SPLINE_CURVE ( 3, ( #1361, #9382, #4155, #8574 ),
 .UNSPECIFIED., .F., .T. ) 
 B_SPLINE_CURVE_WITH_KNOTS ( ( 4, 4 ),
 ( 4.334691002005214955, 4.712388980384689674 ),
 .UNSPECIFIED. ) 
 CURVE ( )  GEOMETRIC_REPRESENTATION_ITEM ( )  RATIONAL_B_SPLINE_CURVE ( ( 1.000000000000000000, 0.9881473088045074071, 0.9881473088045074071, 1.000000000000000000 ) ) 
 REPRESENTATION_ITEM ( '' )  );
#2363 = CARTESIAN_POINT ( 'NONE',  ( 0.7500000000000000000, 0.7500000000000000000, 1.500000000000000000 ) ) ;
#2364 = DIRECTION ( 'NONE',  ( -1.000000000000000000, 0.000000000000000000, 0.000000000000000000 ) ) ;
#2365 = AXIS2_PLACEMENT_3D ( 'NONE', #8680, #5036, #7968 ) ;
#2366 = CARTESIAN_POINT ( 'NONE',  ( 28.00000000000000711, 3.429011037612589670E-15, 10.00000000000000000 ) ) ;
#2367 = PLANE ( 'NONE',  #6747 ) ;
#2368 = LINE ( 'NONE', #2319, #2873 ) ;
#2369 = ADVANCED_FACE ( 'NONE', ( #6264 ), #7595, .F. ) ;
#2370 = CARTESIAN_POINT ( 'NONE',  ( 0.7500000000000000000, 2.749999999999995559, 1.500000000000000000 ) ) ;
#2371 = EDGE_CURVE ( 'NONE', #651, #3742, #6434, .T. ) ;
#2372 = VERTEX_POINT ( 'NONE', #3898 ) ;
#2373 = DIRECTION ( 'NONE',  ( 0.000000000000000000, 0.000000000000000000, -1.000000000000000000 ) ) ;
#2374 = ORIENTED_EDGE ( 'NONE', *, *, #4252, .F. ) ;
#2375 = FACE_OUTER_BOUND ( 'NONE', #2282, .T. ) ;
#2376 = LINE ( 'NONE', #8319, #3952 ) ;
#2377 = CARTESIAN_POINT ( 'NONE',  ( 0.000000000000000000, 34.00000000000001421, 49.50000000000000000 ) ) ;
#2378 = VECTOR ( 'NONE', #276, 1000.000000000000000 ) ;
#2379 = CARTESIAN_POINT ( 'NONE',  ( 0.000000000000000000, -20.00000000000120437, 2.661998082081668380E-12 ) ) ;
#2380 = ORIENTED_EDGE ( 'NONE', *, *, #3656, .F. ) ;
#2381 = CIRCLE ( 'NONE', #2978, 1.000000000000000000 ) ;
#2382 = EDGE_LOOP ( 'NONE', ( #2827, #2922, #8455, #1199 ) ) ;
#2383 = ORIENTED_EDGE ( 'NONE', *, *, #3957, .T. ) ;
#2384 = SHAPE_REPRESENTATION_RELATIONSHIP ( 'NONE' , 'NONE' ,  #1625, #4626 ) ;
#2385 = ORIENTED_EDGE ( 'NONE', *, *, #640, .F. ) ;
#2386 = DIRECTION ( 'NONE',  ( -1.000000000000000000, 0.000000000000000000, 0.000000000000000000 ) ) ;
#2387 = DIRECTION ( 'NONE',  ( -1.000000000000000000, 1.224646799147353454E-16, 0.000000000000000000 ) ) ;
#2388 = CARTESIAN_POINT ( 'NONE',  ( 4.000000000000000000, 7.653668647300657213, -18.47759065022568237 ) ) ;
#2389 = CARTESIAN_POINT ( 'NONE',  ( 0.000000000000000000, 22.50000000000000355, 0.000000000000000000 ) ) ;
#2390 = PLANE ( 'NONE',  #8661 ) ;
#2391 =( GEOMETRIC_REPRESENTATION_CONTEXT ( 3 ) GLOBAL_UNCERTAINTY_ASSIGNED_CONTEXT ( ( #1528 ) ) GLOBAL_UNIT_ASSIGNED_CONTEXT ( ( #5211, #833, #5886 ) ) REPRESENTATION_CONTEXT ( 'NONE', 'WORKASPACE' ) );
#2392 = FACE_OUTER_BOUND ( 'NONE', #7392, .T. ) ;
#2393 = CARTESIAN_POINT ( 'NONE',  ( 27.44426127775442126, -5.090287965588936814, 0.9105965356992768989 ) ) ;
#2394 = ORIENTED_EDGE ( 'NONE', *, *, #6421, .T. ) ;
#2395 = ORIENTED_EDGE ( 'NONE', *, *, #9460, .F. ) ;
#2396 = ORIENTED_EDGE ( 'NONE', *, *, #4998, .F. ) ;
#2397 = FACE_BOUND ( 'NONE', #5749, .T. ) ;
#2398 = CARTESIAN_POINT ( 'NONE',  ( 6.000000000000000888, 7.347880794884120722E-16, 5.000000000000000000 ) ) ;
#2399 = VERTEX_POINT ( 'NONE', #3176 ) ;
#2400 = PLANE ( 'NONE',  #403 ) ;
#2401 = CARTESIAN_POINT ( 'NONE',  ( 1.571166602479410136E-13, -22.50000000000000355, 5.000000000000000000 ) ) ;
#2402 = CARTESIAN_POINT ( 'NONE',  ( 5.000000000000000000, -7.653668647301985040, 18.47759065022880520 ) ) ;
#2403 = UNCERTAINTY_MEASURE_WITH_UNIT (LENGTH_MEASURE( 1.000000000000000082E-05 ), #1011, 'distance_accuracy_value', 'NONE');
#2404 = CARTESIAN_POINT ( 'NONE',  ( -1.335553917663280021, -28.68463450227767453, 1.707979322892793306 ) ) ;
#2405 = VECTOR ( 'NONE', #6335, 1000.000000000000000 ) ;
#2406 = VERTEX_POINT ( 'NONE', #1103 ) ;
#2407 = ORIENTED_EDGE ( 'NONE', *, *, #3115, .F. ) ;
#2408 = DIRECTION ( 'NONE',  ( -0.9711127776881289808, 0.005671107633298151651, 0.2385535821341993323 ) ) ;
#2409 = CARTESIAN_POINT ( 'NONE',  ( 38.00000000000000000, 43.00000000000000000, 11.99999999999999645 ) ) ;
#2410 = DIRECTION ( 'NONE',  ( -0.000000000000000000, -0.000000000000000000, -1.000000000000000000 ) ) ;
#2411 = AXIS2_PLACEMENT_3D ( 'NONE', #7320, #742, #4487 ) ;
#2412 = DIRECTION ( 'NONE',  ( 0.000000000000000000, 0.000000000000000000, -1.000000000000000000 ) ) ;
#2413 = EDGE_CURVE ( 'NONE', #6515, #1161, #4879, .T. ) ;
#2414 = DIRECTION ( 'NONE',  ( -0.7071067811865510144, -0.7071067811865441310, 0.000000000000000000 ) ) ;
#2415 = CARTESIAN_POINT ( 'NONE',  ( 0.000000000000000000, 22.50000000000000355, 5.000000000000000000 ) ) ;
#2416 = VECTOR ( 'NONE', #6409, 1000.000000000000000 ) ;
#2417 = ORIENTED_EDGE ( 'NONE', *, *, #4826, .T. ) ;
#2418 = VECTOR ( 'NONE', #3858, 1000.000000000000000 ) ;
#2419 = FACE_OUTER_BOUND ( 'NONE', #2245, .T. ) ;
#2420 = EDGE_LOOP ( 'NONE', ( #4901, #9272 ) ) ;
#2421 = DIRECTION ( 'NONE',  ( 0.000000000000000000, 1.000000000000000000, 0.000000000000000000 ) ) ;
#2422 = DIRECTION ( 'NONE',  ( 0.000000000000000000, 0.000000000000000000, 1.000000000000000000 ) ) ;
#2423 = VECTOR ( 'NONE', #5957, 1000.000000000000000 ) ;
#2424=STYLED_ITEM('',(#9515),#190);
#2425 = DIRECTION ( 'NONE',  ( -1.000000000000000000, 0.000000000000000000, 0.000000000000000000 ) ) ;
#2426 = VECTOR ( 'NONE', #5054, 1000.000000000000000 ) ;
#2427 = EDGE_CURVE ( 'NONE', #8884, #7524, #8314, .T. ) ;
#2428 = DIRECTION ( 'NONE',  ( -1.000000000000000000, 0.000000000000000000, 0.000000000000000000 ) ) ;
#2429 = CIRCLE ( 'NONE', #7026, 0.7500000000001915135 ) ;
#2430 = EDGE_CURVE ( 'NONE', #2916, #8405, #385, .T. ) ;
#2431 = ORIENTED_EDGE ( 'NONE', *, *, #7296, .T. ) ;
#2432 = ADVANCED_FACE ( 'NONE', ( #2510 ), #342, .F. ) ;
#2433 = EDGE_CURVE ( 'NONE', #3688, #5331, #4954, .T. ) ;
#2434 = ORIENTED_EDGE ( 'NONE', *, *, #5104, .T. ) ;
#2435 = ORIENTED_EDGE ( 'NONE', *, *, #7764, .T. ) ;
#2436 =( LENGTH_UNIT ( ) NAMED_UNIT ( * ) SI_UNIT ( .MILLI., .METRE. ) );
#2437 = VERTEX_POINT ( 'NONE', #4088 ) ;
#2438 = CARTESIAN_POINT ( 'NONE',  ( -53.29490495164537833, -15.90990257669733943, -54.09009742330271564 ) ) ;
#2439 = LINE ( 'NONE', #3197, #1420 ) ;
#2440 = FACE_OUTER_BOUND ( 'NONE', #2337, .T. ) ;
#2441 = VECTOR ( 'NONE', #235, 1000.000000000000114 ) ;
#2442 = DIRECTION ( 'NONE',  ( 0.000000000000000000, 0.000000000000000000, 1.000000000000000000 ) ) ;
#2443 = CARTESIAN_POINT ( 'NONE',  ( -12.37436867076458036, -12.37436867076458036, 19.62563132923542142 ) ) ;
#2444 = PLANE ( 'NONE',  #5337 ) ;
#2445 = DIRECTION ( 'NONE',  ( 1.000000000000000000, 0.000000000000000000, 0.000000000000000000 ) ) ;
#2446 = ADVANCED_FACE ( 'NONE', ( #3999 ), #7021, .F. ) ;
#2447 = ORIENTED_EDGE ( 'NONE', *, *, #8229, .T. ) ;
#2448 = ORIENTED_EDGE ( 'NONE', *, *, #7232, .T. ) ;
#2449 = DIRECTION ( 'NONE',  ( -1.000000000000000000, 0.000000000000000000, 0.000000000000000000 ) ) ;
#2450 = VECTOR ( 'NONE', #1412, 1000.000000000000114 ) ;
#2451 = ORIENTED_EDGE ( 'NONE', *, *, #5657, .F. ) ;
#2452 = EDGE_CURVE ( 'NONE', #8147, #6932, #7920, .T. ) ;
#2453 = FACE_BOUND ( 'NONE', #4235, .T. ) ;
#2454 = VECTOR ( 'NONE', #3090, 1000.000000000000000 ) ;
#2455 = ORIENTED_EDGE ( 'NONE', *, *, #112, .T. ) ;
#2456 = CARTESIAN_POINT ( 'NONE',  ( 2.143131898507868248E-15, 34.00000000000001421, 14.49999999999999822 ) ) ;
#2457 = VECTOR ( 'NONE', #5394, 1000.000000000000114 ) ;
#2458 = DIRECTION ( 'NONE',  ( -1.000000000000000000, 0.000000000000000000, 0.000000000000000000 ) ) ;
#2459 = CARTESIAN_POINT ( 'NONE',  ( 3.614752790974351981, -28.10687131109265735, 1.336560128559570959 ) ) ;
#2460 = ORIENTED_EDGE ( 'NONE', *, *, #2544, .F. ) ;
#2461 = VERTEX_POINT ( 'NONE', #4176 ) ;
#2462 = APPLICATION_PROTOCOL_DEFINITION ( 'draft international standard', 'automotive_design', 1998, #2785 ) ;
#2463 = DIRECTION ( 'NONE',  ( 0.000000000000000000, 0.000000000000000000, -1.000000000000000000 ) ) ;
#2464 = FACE_OUTER_BOUND ( 'NONE', #8608, .T. ) ;
#2465 = DIRECTION ( 'NONE',  ( 0.7071067811865474617, 8.659560562354932858E-17, 0.7071067811865474617 ) ) ;
#2466 = FACE_OUTER_BOUND ( 'NONE', #9297, .T. ) ;
#2467 = CARTESIAN_POINT ( 'NONE',  ( 5.000000000000000000, -7.653668647303860872, -18.47759065022490432 ) ) ;
#2468 = CARTESIAN_POINT ( 'NONE',  ( 8.000000000000021316, 22.50000000000000355, 0.000000000000000000 ) ) ;
#2469 = EDGE_CURVE ( 'NONE', #5629, #5930, #510, .T. ) ;
#2470 = ORIENTED_EDGE ( 'NONE', *, *, #1949, .F. ) ;
#2471 = SURFACE_STYLE_USAGE ( .BOTH. , #2324 ) ;
#2472 = EDGE_LOOP ( 'NONE', ( #3067, #4722, #5397, #1716 ) ) ;
#2473 = CARTESIAN_POINT ( 'NONE',  ( -37.00000000000000000, -21.98223304703364889, -86.98223304703364533 ) ) ;
#2474 = CARTESIAN_POINT ( 'NONE',  ( 3.500000000000000444, -6.505213034913026604E-16, 0.000000000000000000 ) ) ;
#2475 = EDGE_CURVE ( 'NONE', #4866, #5577, #9258, .T. ) ;
#2476 = CARTESIAN_POINT ( 'NONE',  ( 5.000000000000000000, 20.00000000000120437, 7.412591687719288072E-13 ) ) ;
#2477 = CARTESIAN_POINT ( 'NONE',  ( -38.00000000000000711, -43.00000000000000000, -7.366666666666667140 ) ) ;
#2478 = VECTOR ( 'NONE', #5075, 1000.000000000000000 ) ;
#2479 = ORIENTED_EDGE ( 'NONE', *, *, #3239, .F. ) ;
#2480 = APPLICATION_CONTEXT ( 'automotive_design' ) ;
#2481 = VERTEX_POINT ( 'NONE', #8550 ) ;
#2482 = ORIENTED_EDGE ( 'NONE', *, *, #6531, .F. ) ;
#2483 = ORIENTED_EDGE ( 'NONE', *, *, #2543, .F. ) ;
#2484 = CARTESIAN_POINT ( 'NONE',  ( 0.000000000000000000, 14.14213562373247868, 14.14213562373282329 ) ) ;
#2485 = CARTESIAN_POINT ( 'NONE',  ( 22.50000000000000355, 2.356749903719115078E-13, 5.000000000000000000 ) ) ;
#2486 = CARTESIAN_POINT ( 'NONE',  ( -37.00000000000000000, 30.00000000000000000, -78.96446609406727646 ) ) ;
#2487 = CARTESIAN_POINT ( 'NONE',  ( -22.50000000000000000, -7.855833012397050680E-14, 10.00000000000000000 ) ) ;
#2488 = DIRECTION ( 'NONE',  ( 0.000000000000000000, 0.000000000000000000, -1.000000000000000000 ) ) ;
#2489 = CARTESIAN_POINT ( 'NONE',  ( -3.000000000000000000, 22.50000000000000355, 5.000000000000000000 ) ) ;
#2490 = CARTESIAN_POINT ( 'NONE',  ( 0.000000000000000000, -18.47759065022790637, -7.653668647299759265 ) ) ;
#2491 = ORIENTED_EDGE ( 'NONE', *, *, #8177, .T. ) ;
#2492 = VERTEX_POINT ( 'NONE', #1384 ) ;
#2493 = DIRECTION ( 'NONE',  ( -0.000000000000000000, -0.000000000000000000, -1.000000000000000000 ) ) ;
#2494 = ORIENTED_EDGE ( 'NONE', *, *, #5604, .F. ) ;
#2495 = ADVANCED_FACE ( 'NONE', ( #4322 ), #3364, .T. ) ;
#2496 = DIRECTION ( 'NONE',  ( 1.000000000000000000, 1.776356839400250465E-15, 0.000000000000000000 ) ) ;
#2497 = DIRECTION ( 'NONE',  ( 0.000000000000000000, 0.000000000000000000, -1.000000000000000000 ) ) ;
#2498 = VERTEX_POINT ( 'NONE', #7784 ) ;
#2499 = AXIS2_PLACEMENT_3D ( 'NONE', #6357, #2120, #1207 ) ;
#2500 = DIRECTION ( 'NONE',  ( 0.7071067811865460184, 8.659560562354913137E-17, -0.7071067811865489050 ) ) ;
#2501 = FACE_OUTER_BOUND ( 'NONE', #2382, .T. ) ;
#2502 = CARTESIAN_POINT ( 'NONE',  ( 0.3423334138323023135, -28.74982858564768762, 1.749889805059230419 ) ) ;
#2503 = VERTEX_POINT ( 'NONE', #521 ) ;
#2504 = EDGE_LOOP ( 'NONE', ( #173, #3409, #7269, #6350 ) ) ;
#2505 = AXIS2_PLACEMENT_3D ( 'NONE', #6684, #8086, #778 ) ;
#2506 = CARTESIAN_POINT ( 'NONE',  ( 15.70011763207405231, -9.048619709455117288, 47.70011763207405409 ) ) ;
#2507 = CARTESIAN_POINT ( 'NONE',  ( 0.000000000000000000, -22.50000000000000355, 5.000000000000000000 ) ) ;
#2508 = DIRECTION ( 'NONE',  ( -0.7071067811865441310, 0.7071067811865510144, -0.000000000000000000 ) ) ;
#2509 = LINE ( 'NONE', #341, #726 ) ;
#2510 = FACE_OUTER_BOUND ( 'NONE', #1727, .T. ) ;
#2511 = ORIENTED_EDGE ( 'NONE', *, *, #9181, .T. ) ;
#2512 = CARTESIAN_POINT ( 'NONE',  ( -3.500000000000000000, 4.119968255444916849E-15, 0.000000000000000000 ) ) ;
#2513 = ORIENTED_EDGE ( 'NONE', *, *, #8827, .T. ) ;
#2514 = CARTESIAN_POINT ( 'NONE',  ( 32.00000000000000711, 29.99999999999997868, 5.000000000000031974 ) ) ;
#2515 = DIRECTION ( 'NONE',  ( 1.000000000000000000, 0.000000000000000000, 0.000000000000000000 ) ) ;
#2516 = CIRCLE ( 'NONE', #5273, 16.00000000000000000 ) ;
#2517 = CARTESIAN_POINT ( 'NONE',  ( 0.000000000000000000, 7.653668647302530381, 17.72759065022973246 ) ) ;
#2518 = EDGE_CURVE ( 'NONE', #2159, #6631, #8636, .T. ) ;
#2519 = CYLINDRICAL_SURFACE ( 'NONE', #1400, 11.00000000000000000 ) ;
#2520 = ORIENTED_EDGE ( 'NONE', *, *, #1589, .F. ) ;
#2521 = ORIENTED_EDGE ( 'NONE', *, *, #1023, .T. ) ;
#2522 = EDGE_CURVE ( 'NONE', #2562, #1694, #1992, .T. ) ;
#2523 = VERTEX_POINT ( 'NONE', #1283 ) ;
#2524 = ORIENTED_EDGE ( 'NONE', *, *, #7908, .T. ) ;
#2525 = CARTESIAN_POINT ( 'NONE',  ( -52.86930915046636414, -28.38475884032111196, -81.18159060786256020 ) ) ;
#2526 = FACE_OUTER_BOUND ( 'NONE', #8135, .T. ) ;
#2527 = DIRECTION ( 'NONE',  ( 0.7071067811865507924, 0.7071067811865441310, -0.000000000000000000 ) ) ;
#2528 = CIRCLE ( 'NONE', #224, 3.000000000000000444 ) ;
#2529 = LINE ( 'NONE', #1122, #8459 ) ;
#2530 = VECTOR ( 'NONE', #545, 1000.000000000000000 ) ;
#2531 = CARTESIAN_POINT ( 'NONE',  ( 0.000000000000000000, -14.14213562373248401, -14.14213562372942157 ) ) ;
#2532 = CARTESIAN_POINT ( 'NONE',  ( 26.42320443315922063, -6.702656137449844564, 0.2542028498880765097 ) ) ;
#2533 = EDGE_CURVE ( 'NONE', #6932, #3553, #1197, .T. ) ;
#2534 = EDGE_LOOP ( 'NONE', ( #5986, #5234 ) ) ;
#2535 = ORIENTED_EDGE ( 'NONE', *, *, #2941, .T. ) ;
#2536 = FACE_BOUND ( 'NONE', #9197, .T. ) ;
#2537 = VERTEX_POINT ( 'NONE', #7830 ) ;
#2538 = FACE_BOUND ( 'NONE', #9289, .T. ) ;
#2539 = DIRECTION ( 'NONE',  ( 0.000000000000000000, 1.000000000000000000, 0.000000000000000000 ) ) ;
#2540 = AXIS2_PLACEMENT_3D ( 'NONE', #7395, #3750, #7352 ) ;
#2541 = ORIENTED_EDGE ( 'NONE', *, *, #2177, .T. ) ;
#2542 = CARTESIAN_POINT ( 'NONE',  ( 5.000000000000000000, -9.626277053524975217E-13, -21.56000000000076966 ) ) ;
#2543 = EDGE_CURVE ( 'NONE', #7343, #1832, #477, .T. ) ;
#2544 = EDGE_CURVE ( 'NONE', #1969, #6082, #9407, .T. ) ;
#2545 = CARTESIAN_POINT ( 'NONE',  ( 0.000000000000000000, 0.000000000000000000, 10.00000000000000000 ) ) ;
#2546 = CARTESIAN_POINT ( 'NONE',  ( 60.00000000000000000, 15.90990257669733943, -85.90990257669729147 ) ) ;
#2547 = ORIENTED_EDGE ( 'NONE', *, *, #6826, .F. ) ;
#2548 = ORIENTED_EDGE ( 'NONE', *, *, #331, .T. ) ;
#2549 = ADVANCED_FACE ( 'NONE', ( #2016, #1239 ), #7063, .T. ) ;
#2550 = EDGE_CURVE ( 'NONE', #5750, #3148, #807, .T. ) ;
#2551 = AXIS2_PLACEMENT_3D ( 'NONE', #9049, #7463, #4639 ) ;
#2552 = CYLINDRICAL_SURFACE ( 'NONE', #6568, 3.000000000000000000 ) ;
#2553 = CARTESIAN_POINT ( 'NONE',  ( 0.000000000000000000, 0.000000000000000000, 25.00000000000000000 ) ) ;
#2554 = AXIS2_PLACEMENT_3D ( 'NONE', #7004, #2463, #413 ) ;
#2555 = SURFACE_STYLE_FILL_AREA ( #1875 ) ;
#2556 = DIRECTION ( 'NONE',  ( 0.000000000000000000, -1.000000000000000000, 0.000000000000000000 ) ) ;
#2557 = EDGE_CURVE ( 'NONE', #8610, #4346, #6447, .T. ) ;
#2558 = DIRECTION ( 'NONE',  ( 1.000000000000000000, 0.000000000000000000, -0.000000000000000000 ) ) ;
#2559 = ADVANCED_FACE ( 'NONE', ( #1921 ), #3424, .F. ) ;
#2560 = ORIENTED_EDGE ( 'NONE', *, *, #5065, .T. ) ;
#2561 = CARTESIAN_POINT ( 'NONE',  ( -37.00000000000000000, -30.00000000000000000, -95.00000000000000000 ) ) ;
#2562 = VERTEX_POINT ( 'NONE', #622 ) ;
#2563 = ADVANCED_FACE ( 'NONE', ( #6395 ), #8594, .F. ) ;
#2564 = AXIS2_PLACEMENT_3D ( 'NONE', #5991, #6039, #8194 ) ;
#2565 = FACE_OUTER_BOUND ( 'NONE', #1909, .T. ) ;
#2566 = CARTESIAN_POINT ( 'NONE',  ( 0.7500000000000000000, -0.7500000000000000000, 0.000000000000000000 ) ) ;
#2567 = CARTESIAN_POINT ( 'NONE',  ( 15.70011763207405586, 9.048619709455111959, 16.29988236792594591 ) ) ;
#2568 = CARTESIAN_POINT ( 'NONE',  ( 39.50000000000000000, 29.99999999999999645, -82.50000000000000000 ) ) ;
#2569 = CLOSED_SHELL ( 'NONE', ( #475, #9166, #5459, #8347, #8526, #4360, #1775, #2703, #6052, #1140, #5949, #1308, #1593, #238, #4738, #3143, #311, #3299, #8357, #7241, #8471, #4044, #1954, #9270, #3261, #7014, #8345, #3241, #4710, #8473, #2720, #1290, #1887, #1314, #7688, #42, #1539, #5048, #2161, #3947, #4916, #8528, #255, #6151, #4509, #7208, #5630 ) ) ;
#2570 = AXIS2_PLACEMENT_3D ( 'NONE', #2327, #3810, #3276 ) ;
#2571 = VECTOR ( 'NONE', #867, 1000.000000000000000 ) ;
#2572 = EDGE_LOOP ( 'NONE', ( #2470, #6825 ) ) ;
#2573 = VERTEX_POINT ( 'NONE', #8641 ) ;
#2574 = VERTEX_POINT ( 'NONE', #4220 ) ;
#2575 = AXIS2_PLACEMENT_3D ( 'NONE', #93, #6535, #51 ) ;
#2576 = DIRECTION ( 'NONE',  ( -1.000000000000000000, 0.000000000000000000, 0.000000000000000000 ) ) ;
#2577 = DIRECTION ( 'NONE',  ( 0.000000000000000000, 0.000000000000000000, -1.000000000000000000 ) ) ;
#2578 = VECTOR ( 'NONE', #7350, 1000.000000000000000 ) ;
#2579 = LINE ( 'NONE', #3976, #26 ) ;
#2580 = CIRCLE ( 'NONE', #2106, 12.50000000000000000 ) ;
#2581 = CARTESIAN_POINT ( 'NONE',  ( -15.70011763207405231, -9.048619709455117288, 47.70011763207404698 ) ) ;
#2582 = CYLINDRICAL_SURFACE ( 'NONE', #4355, 6.000000000000001776 ) ;
#2583 = CIRCLE ( 'NONE', #579, 17.50000000000000355 ) ;
#2584 = VERTEX_POINT ( 'NONE', #7150 ) ;
#2585 = ORIENTED_EDGE ( 'NONE', *, *, #9139, .F. ) ;
#2586 = CARTESIAN_POINT ( 'NONE',  ( -2.750000000000002665, -0.7500000000000000000, 0.000000000000000000 ) ) ;
#2587 = ORIENTED_EDGE ( 'NONE', *, *, #4299, .F. ) ;
#2588 = PLANE ( 'NONE',  #957 ) ;
#2589 = CARTESIAN_POINT ( 'NONE',  ( 19.74999999999999645, 43.00000000000000000, 25.00000000000000000 ) ) ;
#2590 = AXIS2_PLACEMENT_3D ( 'NONE', #4607, #285, #7679 ) ;
#2591 = EDGE_LOOP ( 'NONE', ( #882, #5563, #8324, #7902 ) ) ;
#2592 = DIRECTION ( 'NONE',  ( 0.000000000000000000, -1.000000000000000000, 0.000000000000000000 ) ) ;
#2593 = VECTOR ( 'NONE', #7371, 1000.000000000000000 ) ;
#2594 = FACE_OUTER_BOUND ( 'NONE', #3889, .T. ) ;
#2595 = VECTOR ( 'NONE', #935, 1000.000000000000000 ) ;
#2596 = CYLINDRICAL_SURFACE ( 'NONE', #4572, 1.560000000001466436 ) ;
#2597 = ORIENTED_EDGE ( 'NONE', *, *, #7344, .T. ) ;
#2598 = CIRCLE ( 'NONE', #3520, 3.000000000000002665 ) ;
#2599 = VERTEX_POINT ( 'NONE', #573 ) ;
#2600 = EDGE_CURVE ( 'NONE', #9251, #9218, #7246, .T. ) ;
#2601 = AXIS2_PLACEMENT_3D ( 'NONE', #160, #3082, #5146 ) ;
#2602 = CARTESIAN_POINT ( 'NONE',  ( 3.500000000000000444, -2.818925648462311528E-15, 0.000000000000000000 ) ) ;
#2603 = EDGE_CURVE ( 'NONE', #7596, #4808, #1431, .T. ) ;
#2604 = EDGE_CURVE ( 'NONE', #8987, #6860, #2920, .T. ) ;
#2605 = ADVANCED_FACE ( 'NONE', ( #8164 ), #5857, .F. ) ;
#2606 = PLANE ( 'NONE',  #80 ) ;
#2607 = CARTESIAN_POINT ( 'NONE',  ( 5.000000000000000000, 14.14213562373112154, -15.70213562373078098 ) ) ;
#2608 = CARTESIAN_POINT ( 'NONE',  ( -27.73557521625266276, 4.508354841688235304, 1.097869781876724238 ) ) ;
#2609 = ORIENTED_EDGE ( 'NONE', *, *, #1362, .F. ) ;
#2610 = PLANE ( 'NONE',  #5341 ) ;
#2611 = ORIENTED_EDGE ( 'NONE', *, *, #3601, .T. ) ;
#2612 = DIRECTION ( 'NONE',  ( 0.000000000000000000, -1.000000000000000000, 0.000000000000000000 ) ) ;
#2613 = CYLINDRICAL_SURFACE ( 'NONE', #5650, 11.00000000000000711 ) ;
#2614 = CARTESIAN_POINT ( 'NONE',  ( 0.000000000000000000, -35.00000000000000000, 32.00000000000000000 ) ) ;
#2615 = CIRCLE ( 'NONE', #1675, 11.00000000000000711 ) ;
#2616 =( BOUNDED_CURVE ( )  B_SPLINE_CURVE ( 3, ( #7588, #3170, #2506, #3795 ),
 .UNSPECIFIED., .F., .F. ) 
 B_SPLINE_CURVE_WITH_KNOTS ( ( 4, 4 ),
 ( 0.000000000000000000, 0.7853981633974485010 ),
 .UNSPECIFIED. ) 
 CURVE ( )  GEOMETRIC_REPRESENTATION_ITEM ( )  RATIONAL_B_SPLINE_CURVE ( ( 1.000000000000000000, 0.9492530216741911220, 0.9492530216741911220, 1.000000000000000000 ) ) 
 REPRESENTATION_ITEM ( '' )  );
#2617 = DIRECTION ( 'NONE',  ( -0.000000000000000000, -0.000000000000000000, -1.000000000000000000 ) ) ;
#2618 = ADVANCED_FACE ( 'NONE', ( #5955 ), #712, .T. ) ;
#2619 = ORIENTED_EDGE ( 'NONE', *, *, #7810, .F. ) ;
#2620 = ORIENTED_EDGE ( 'NONE', *, *, #2901, .T. ) ;
#2621 = DIRECTION ( 'NONE',  ( 9.495567745759693325E-66, 0.9997175446104182850, -0.02376617340079601251 ) ) ;
#2622 = VERTEX_POINT ( 'NONE', #8782 ) ;
#2623 = DIRECTION ( 'NONE',  ( 1.000000000000000000, 0.000000000000000000, 0.000000000000000000 ) ) ;
#2624 = EDGE_CURVE ( 'NONE', #6868, #1832, #4267, .T. ) ;
#2625 = VECTOR ( 'NONE', #3927, 1000.000000000000000 ) ;
#2626 = DIRECTION ( 'NONE',  ( -1.000000000000000000, 0.000000000000000000, -0.000000000000000000 ) ) ;
#2627 = VECTOR ( 'NONE', #2592, 1000.000000000000000 ) ;
#2628 = DIRECTION ( 'NONE',  ( 1.000000000000000000, -0.000000000000000000, -0.000000000000000000 ) ) ;
#2629 = CARTESIAN_POINT ( 'NONE',  ( 26.91700667250950829, 4.077589154199230848, 0.2225055604246540530 ) ) ;
#2630 = DIRECTION ( 'NONE',  ( -1.000000000000000000, -0.000000000000000000, -0.000000000000000000 ) ) ;
#2631 = ORIENTED_EDGE ( 'NONE', *, *, #9056, .F. ) ;
#2632 = ORIENTED_EDGE ( 'NONE', *, *, #700, .F. ) ;
#2633 = CARTESIAN_POINT ( 'NONE',  ( -15.99999999999999645, 43.00000000000000000, -7.366666666666667140 ) ) ;
#2634 = AXIS2_PLACEMENT_3D ( 'NONE', #4062, #6906, #6143 ) ;
#2635 = VERTEX_POINT ( 'NONE', #7290 ) ;
#2636 = CARTESIAN_POINT ( 'NONE',  ( 0.000000000000000000, 7.653668647302530381, 18.47759065022802716 ) ) ;
#2637 = DIRECTION ( 'NONE',  ( 0.000000000000000000, 0.000000000000000000, 1.000000000000000000 ) ) ;
#2638 = VERTEX_POINT ( 'NONE', #6676 ) ;
#2639 = FACE_OUTER_BOUND ( 'NONE', #6449, .T. ) ;
#2640 = CARTESIAN_POINT ( 'NONE',  ( 26.21170834203230982, 53.97171801779368394, -0.5000000000000038858 ) ) ;
#2641 = ADVANCED_FACE ( 'NONE', ( #50 ), #9415, .F. ) ;
#2642 = DIRECTION ( 'NONE',  ( 1.000000000000000000, -0.000000000000000000, -0.000000000000000000 ) ) ;
#2643 = CARTESIAN_POINT ( 'NONE',  ( 28.10782586465402488, 3.612161042402800781, 1.337173770134738371 ) ) ;
#2644 = ORIENTED_EDGE ( 'NONE', *, *, #5753, .T. ) ;
#2645 = EDGE_LOOP ( 'NONE', ( #3021, #5451, #1726, #6636 ) ) ;
#2646 = AXIS2_PLACEMENT_3D ( 'NONE', #2330, #5882, #2945 ) ;
#2647 = EDGE_CURVE ( 'NONE', #4404, #7651, #7426, .T. ) ;
#2648 = ITEM_DEFINED_TRANSFORMATION ( 'NONE', 'NONE', #2225,  #1614 ) ;
#2649 = DIRECTION ( 'NONE',  ( 0.000000000000000000, 0.000000000000000000, -1.000000000000000000 ) ) ;
#2650 = AXIS2_PLACEMENT_3D ( 'NONE', #3704, #4517, #6786 ) ;
#2651 = CARTESIAN_POINT ( 'NONE',  ( -25.50000000000000000, -7.855833012397050680E-14, 5.000000000000000000 ) ) ;
#2652 = DIRECTION ( 'NONE',  ( -0.000000000000000000, -0.000000000000000000, -1.000000000000000000 ) ) ;
#2653 = DIRECTION ( 'NONE',  ( 0.000000000000000000, -1.000000000000000000, 0.000000000000000000 ) ) ;
#2654 = ORIENTED_EDGE ( 'NONE', *, *, #640, .T. ) ;
#2655 = CIRCLE ( 'NONE', #6337, 60.00000000000000000 ) ;
#2656 = EDGE_LOOP ( 'NONE', ( #7957, #9298 ) ) ;
#2657 = ORIENTED_EDGE ( 'NONE', *, *, #1402, .T. ) ;
#2658 = PLANE ( 'NONE',  #200 ) ;
#2659 =( REPRESENTATION_RELATIONSHIP ('NONE','NONE', #1933, #8501 ) REPRESENTATION_RELATIONSHIP_WITH_TRANSFORMATION ( #6391 )SHAPE_REPRESENTATION_RELATIONSHIP( ) );
#2660 = LINE ( 'NONE', #4859, #5017 ) ;
#2661 = AXIS2_PLACEMENT_3D ( 'NONE', #3517, #1258, #6283 ) ;
#2662 = CARTESIAN_POINT ( 'NONE',  ( -60.00000000000000000, -30.00000000000000000, -13.00000000000000000 ) ) ;
#2663 = ADVANCED_FACE ( 'NONE', ( #8066 ), #4416, .F. ) ;
#2664 = CARTESIAN_POINT ( 'NONE',  ( -37.00000000000000711, -15.90990257669733943, -57.09009742330271564 ) ) ;
#2665 = ADVANCED_FACE ( 'NONE', ( #7338, #2, #4506, #8738, #8881, #2154 ), #2200, .T. ) ;
#2666 = ORIENTED_EDGE ( 'NONE', *, *, #1428, .F. ) ;
#2667 = ORIENTED_EDGE ( 'NONE', *, *, #8210, .T. ) ;
#2668 = DIRECTION ( 'NONE',  ( 0.000000000000000000, -0.5535840618632023036, -0.8327933035579949683 ) ) ;
#2669 = EDGE_LOOP ( 'NONE', ( #138, #6352 ) ) ;
#2670 = DIRECTION ( 'NONE',  ( 1.224646799147353207E-16, 1.000000000000000000, -0.000000000000000000 ) ) ;
#2671 = AXIS2_PLACEMENT_3D ( 'NONE', #6209, #7549, #2558 ) ;
#2672 = DIRECTION ( 'NONE',  ( -1.000000000000000000, -0.000000000000000000, -0.000000000000000000 ) ) ;
#2673 = DIRECTION ( 'NONE',  ( 0.000000000000000000, 0.000000000000000000, -1.000000000000000000 ) ) ;
#2674 = CARTESIAN_POINT ( 'NONE',  ( 60.00000000000000000, 15.90990257669733943, -85.90990257669729147 ) ) ;
#2675 = DIRECTION ( 'NONE',  ( 0.000000000000000000, -1.000000000000000000, 0.000000000000000000 ) ) ;
#2676 = ORIENTED_EDGE ( 'NONE', *, *, #5228, .F. ) ;
#2677 = VERTEX_POINT ( 'NONE', #8207 ) ;
#2678 = DIRECTION ( 'NONE',  ( -0.000000000000000000, -0.000000000000000000, 1.000000000000000000 ) ) ;
#2679 = ORIENTED_EDGE ( 'NONE', *, *, #2214, .F. ) ;
#2680 = CARTESIAN_POINT ( 'NONE',  ( 0.000000000000000000, 0.000000000000000000, 4.000000000000000000 ) ) ;
#2681 = CARTESIAN_POINT ( 'NONE',  ( -37.00000000000000000, -30.00000000000000000, -95.00000000000000000 ) ) ;
#2682 = CARTESIAN_POINT ( 'NONE',  ( -0.7500000000000000000, -0.7500000000000000000, 0.000000000000000000 ) ) ;
#2683 = VECTOR ( 'NONE', #3152, 1000.000000000000000 ) ;
#2684 = DIRECTION ( 'NONE',  ( -0.000000000000000000, -1.000000000000000000, -0.000000000000000000 ) ) ;
#2685 = VECTOR ( 'NONE', #8053, 1000.000000000000000 ) ;
#2686 = DIRECTION ( 'NONE',  ( 1.000000000000000000, 0.000000000000000000, 0.000000000000000000 ) ) ;
#2687 = DIRECTION ( 'NONE',  ( -0.000000000000000000, -0.000000000000000000, -1.000000000000000000 ) ) ;
#2688 = VERTEX_POINT ( 'NONE', #852 ) ;
#2689 = CIRCLE ( 'NONE', #1292, 3.000000000000002665 ) ;
#2690 = VERTEX_POINT ( 'NONE', #5231 ) ;
#2691 = CONTEXT_DEPENDENT_SHAPE_REPRESENTATION ( #4752, #6392 ) ;
#2692 = PLANE ( 'NONE',  #6831 ) ;
#2693 = CARTESIAN_POINT ( 'NONE',  ( 22.50000000000000355, 2.356749903719115078E-13, 10.00000000000000000 ) ) ;
#2694 = LINE ( 'NONE', #1338, #275 ) ;
#2695 = PRODUCT_DEFINITION_FORMATION_WITH_SPECIFIED_SOURCE ( 'ANY', '', #6699, .NOT_KNOWN. ) ;
#2696 = ORIENTED_EDGE ( 'NONE', *, *, #135, .T. ) ;
#2697 = VERTEX_POINT ( 'NONE', #7434 ) ;
#2698 = ORIENTED_EDGE ( 'NONE', *, *, #4937, .T. ) ;
#2699 = ORIENTED_EDGE ( 'NONE', *, *, #9216, .T. ) ;
#2700 = DIRECTION ( 'NONE',  ( 0.000000000000000000, -1.000000000000000000, 0.000000000000000000 ) ) ;
#2701 = CARTESIAN_POINT ( 'NONE',  ( -38.00000000000000711, -20.99999999999999289, -16.89999999999999858 ) ) ;
#2702 = AXIS2_PLACEMENT_3D ( 'NONE', #1988, #2033, #8021 ) ;
#2703 = ADVANCED_FACE ( 'NONE', ( #3691 ), #6628, .F. ) ;
#2704 = CARTESIAN_POINT ( 'NONE',  ( -37.00000000000000711, -15.90990257669733943, -54.09009742330271564 ) ) ;
#2705 = PRODUCT ( '4-Axle(Cross)', '4-Axle(Cross)', '', ( #9117 ) ) ;
#2706 = CARTESIAN_POINT ( 'NONE',  ( -28.48725673979378570, -2.337639529181975817, 1.581093618438872195 ) ) ;
#2707 = PLANE ( 'NONE',  #2264 ) ;
#2708 = ORIENTED_EDGE ( 'NONE', *, *, #6531, .T. ) ;
#2709 = CIRCLE ( 'NONE', #855, 1.559999999999096776 ) ;
#2710 = ORIENTED_EDGE ( 'NONE', *, *, #5371, .F. ) ;
#2711 = EDGE_LOOP ( 'NONE', ( #4423, #8156 ) ) ;
#2712 = DIRECTION ( 'NONE',  ( 1.000000000000000000, 0.000000000000000000, 0.000000000000000000 ) ) ;
#2713 = CARTESIAN_POINT ( 'NONE',  ( -28.45342843414351108, 0.8561988828942436180, 1.463295953604768496 ) ) ;
#2714 = ADVANCED_FACE ( 'NONE', ( #8120, #1527, #7387, #2355, #6731, #149 ), #1050, .T. ) ;
#2715 = AXIS2_PLACEMENT_3D ( 'NONE', #7213, #6554, #8753 ) ;
#2716 = FACE_OUTER_BOUND ( 'NONE', #1555, .T. ) ;
#2717 = EDGE_CURVE ( 'NONE', #6270, #4692, #4577, .T. ) ;
#2718 = DIRECTION ( 'NONE',  ( -0.7071067811865426878, 0.000000000000000000, -0.7071067811865524577 ) ) ;
#2719 = EDGE_CURVE ( 'NONE', #6045, #7524, #3900, .T. ) ;
#2720 = ADVANCED_FACE ( 'NONE', ( #1724 ), #193, .F. ) ;
#2721 = DIRECTION ( 'NONE',  ( -0.000000000000000000, -0.000000000000000000, -1.000000000000000000 ) ) ;
#2722 = EDGE_LOOP ( 'NONE', ( #1918, #2252, #4757, #785 ) ) ;
#2723 = AXIS2_PLACEMENT_3D ( 'NONE', #2063, #2653, #4854 ) ;
#2724 = EDGE_LOOP ( 'NONE', ( #7156, #3318, #2511, #1507 ) ) ;
#2725 = DIRECTION ( 'NONE',  ( 0.000000000000000000, 0.000000000000000000, -1.000000000000000000 ) ) ;
#2726 =( GEOMETRIC_REPRESENTATION_CONTEXT ( 3 ) GLOBAL_UNCERTAINTY_ASSIGNED_CONTEXT ( ( #7486 ) ) GLOBAL_UNIT_ASSIGNED_CONTEXT ( ( #3038, #6790, #5976 ) ) REPRESENTATION_CONTEXT ( 'NONE', 'WORKASPACE' ) );
#2727 = VERTEX_POINT ( 'NONE', #3838 ) ;
#2728 = CARTESIAN_POINT ( 'NONE',  ( 0.000000000000000000, 22.50000000000000355, 10.00000000000000000 ) ) ;
#2729 = DIRECTION ( 'NONE',  ( -1.000000000000000000, 0.000000000000000000, 0.000000000000000000 ) ) ;
#2730 =( BOUNDED_CURVE ( )  B_SPLINE_CURVE ( 3, ( #2897, #4291, #3613, #9376 ),
 .UNSPECIFIED., .F., .F. ) 
 B_SPLINE_CURVE_WITH_KNOTS ( ( 4, 4 ),
 ( 2.356194490192344837, 3.141592653589793116 ),
 .UNSPECIFIED. ) 
 CURVE ( )  GEOMETRIC_REPRESENTATION_ITEM ( )  RATIONAL_B_SPLINE_CURVE ( ( 1.000000000000000000, 0.9492530216741911220, 0.9492530216741911220, 1.000000000000000000 ) ) 
 REPRESENTATION_ITEM ( '' )  );
#2731 = DIRECTION ( 'NONE',  ( 0.000000000000000000, 1.000000000000000000, 0.000000000000000000 ) ) ;
#2732 = AXIS2_PLACEMENT_3D ( 'NONE', #4274, #8064, #2014 ) ;
#2733 = CARTESIAN_POINT ( 'NONE',  ( 3.000000000000000000, 22.50000000000000355, 5.000000000000000000 ) ) ;
#2734 = CIRCLE ( 'NONE', #6275, 11.96410161513786008 ) ;
#2735 = CIRCLE ( 'NONE', #9012, 2.999999999999999112 ) ;
#2736 = B_SPLINE_CURVE_WITH_KNOTS ( 'NONE', 3,
 ( #8484, #2629, #1081, #5559, #1803, #8334, #3201, #1898, #1217, #6907, #8441, #4691 ),
 .UNSPECIFIED., .F., .F.,
 ( 4, 2, 2, 2, 2, 4 ),
 ( 0.000000000000000000, 0.001279392565614386563, 0.002558785131228773126, 0.003838177696843159473, 0.004477873979650353296, 0.005117570262457546253 ),
 .UNSPECIFIED. ) ;
#2737 = DIRECTION ( 'NONE',  ( 0.000000000000000000, 0.000000000000000000, -1.000000000000000000 ) ) ;
#2738 = PLANE ( 'NONE',  #122 ) ;
#2739 = EDGE_CURVE ( 'NONE', #6084, #4903, #8401, .T. ) ;
#2740 = ORIENTED_EDGE ( 'NONE', *, *, #553, .T. ) ;
#2741 = EDGE_LOOP ( 'NONE', ( #198, #493, #1242, #3924 ) ) ;
#2742 = VECTOR ( 'NONE', #7286, 1000.000000000000000 ) ;
#2743 = ADVANCED_FACE ( 'NONE', ( #3164 ), #3259, .T. ) ;
#2744 = DIRECTION ( 'NONE',  ( 1.000000000000000000, 0.000000000000000000, 0.000000000000000000 ) ) ;
#2745 = AXIS2_PLACEMENT_3D ( 'NONE', #5842, #6661, #8769 ) ;
#2746 = LINE ( 'NONE', #3401, #528 ) ;
#2747 = CARTESIAN_POINT ( 'NONE',  ( -58.90150666944372659, 9.142135623730833771, -91.89339828220165884 ) ) ;
#2748 = DIRECTION ( 'NONE',  ( -0.000000000000000000, -0.000000000000000000, -1.000000000000000000 ) ) ;
#2749 = EDGE_LOOP ( 'NONE', ( #2898, #7997 ) ) ;
#2750 = EDGE_LOOP ( 'NONE', ( #1953, #3829, #8681 ) ) ;
#2751 = EDGE_LOOP ( 'NONE', ( #2906, #3966 ) ) ;
#2752 = AXIS2_PLACEMENT_3D ( 'NONE', #2000, #7089, #9198 ) ;
#2753 = ORIENTED_EDGE ( 'NONE', *, *, #895, .T. ) ;
#2754 = AXIS2_PLACEMENT_3D ( 'NONE', #8950, #2329, #5259 ) ;
#2755 = DIRECTION ( 'NONE',  ( 1.000000000000000000, 0.000000000000000000, -0.000000000000000000 ) ) ;
#2756 = DIRECTION ( 'NONE',  ( -1.000000000000000000, -0.000000000000000000, -0.000000000000000000 ) ) ;
#2757 = DIRECTION ( 'NONE',  ( 0.000000000000000000, -0.7071067811865473507, -0.7071067811865477948 ) ) ;
#2758 = CARTESIAN_POINT ( 'NONE',  ( -26.02777777777775370, -7.180166011355047395, 0.000000000000000000 ) ) ;
#2759 = ADVANCED_FACE ( 'NONE', ( #2594 ), #673, .F. ) ;
#2760 = DIRECTION ( 'NONE',  ( 0.000000000000000000, 0.000000000000000000, -1.000000000000000000 ) ) ;
#2761 = ORIENTED_EDGE ( 'NONE', *, *, #2944, .T. ) ;
#2762 = EDGE_LOOP ( 'NONE', ( #4778, #5471, #8447, #6329 ) ) ;
#2763 = DIRECTION ( 'NONE',  ( 1.000000000000000000, 0.000000000000000000, 0.000000000000000000 ) ) ;
#2764 = ORIENTED_EDGE ( 'NONE', *, *, #1661, .F. ) ;
#2765 = DIRECTION ( 'NONE',  ( 1.000000000000000000, 0.000000000000000000, 0.000000000000000000 ) ) ;
#2766 = EDGE_CURVE ( 'NONE', #6634, #4866, #1280, .T. ) ;
#2767 = DIRECTION ( 'NONE',  ( 1.000000000000000000, 0.000000000000000000, 0.000000000000000000 ) ) ;
#2768 = LINE ( 'NONE', #7949, #4312 ) ;
#2769 = CARTESIAN_POINT ( 'NONE',  ( -22.50000000000000355, 0.000000000000000000, 5.000000000000000000 ) ) ;
#2770 = LINE ( 'NONE', #8486, #7735 ) ;
#2771 = ORIENTED_EDGE ( 'NONE', *, *, #21, .T. ) ;
#2772 = VERTEX_POINT ( 'NONE', #6247 ) ;
#2773 = CYLINDRICAL_SURFACE ( 'NONE', #4093, 2.999999999999999112 ) ;
#2774 = EDGE_LOOP ( 'NONE', ( #5885, #9364 ) ) ;
#2775 = DIRECTION ( 'NONE',  ( 1.000000000000000000, 0.000000000000000000, 0.000000000000000000 ) ) ;
#2776 = DIRECTION ( 'NONE',  ( 0.000000000000000000, 0.000000000000000000, -1.000000000000000000 ) ) ;
#2777 = LINE ( 'NONE', #5665, #3930 ) ;
#2778 = FACE_OUTER_BOUND ( 'NONE', #5610, .T. ) ;
#2779 = CYLINDRICAL_SURFACE ( 'NONE', #5124, 17.50000000000000000 ) ;
#2780 = AXIS2_PLACEMENT_3D ( 'NONE', #2290, #1565, #1464 ) ;
#2781 = CARTESIAN_POINT ( 'NONE',  ( 5.000000000000000000, 7.653668647300657213, -17.72759065022447089 ) ) ;
#2782 = ADVANCED_FACE ( 'NONE', ( #4610 ), #1768, .F. ) ;
#2783 = EDGE_LOOP ( 'NONE', ( #7771, #7752, #7346, #5312, #2111 ) ) ;
#2784 = ORIENTED_EDGE ( 'NONE', *, *, #462, .T. ) ;
#2785 = APPLICATION_CONTEXT ( 'automotive_design' ) ;
#2786 = CARTESIAN_POINT ( 'NONE',  ( -22.50000000000000000, -7.855833012397050680E-14, 5.000000000000000000 ) ) ;
#2787 = CARTESIAN_POINT ( 'NONE',  ( 19.74999999999999645, -43.00000000000000000, 11.99999999999999645 ) ) ;
#2788 = DIRECTION ( 'NONE',  ( 0.7071067811865460184, 0.000000000000000000, -0.7071067811865489050 ) ) ;
#2789 = LINE ( 'NONE', #5724, #4409 ) ;
#2790 = CIRCLE ( 'NONE', #1870, 17.50000000000000000 ) ;
#2791 = ORIENTED_EDGE ( 'NONE', *, *, #4233, .F. ) ;
#2792 = EDGE_LOOP ( 'NONE', ( #8710, #1524, #8498, #123, #5111 ) ) ;
#2793 = ORIENTED_EDGE ( 'NONE', *, *, #7323, .T. ) ;
#2794 = EDGE_LOOP ( 'NONE', ( #2110, #6691, #8786, #3108 ) ) ;
#2795 = DIRECTION ( 'NONE',  ( -0.000000000000000000, -0.000000000000000000, -1.000000000000000000 ) ) ;
#2796 = AXIS2_PLACEMENT_3D ( 'NONE', #5639, #8562, #1984 ) ;
#2797 = CARTESIAN_POINT ( 'NONE',  ( 0.000000000000000000, 0.000000000000000000, 5.000000000000000000 ) ) ;
#2798 = DIRECTION ( 'NONE',  ( 0.000000000000000000, 0.000000000000000000, 1.000000000000000000 ) ) ;
#2799 = CARTESIAN_POINT ( 'NONE',  ( -28.73308667824889540, -0.6789743538665677924, 1.739127150302868463 ) ) ;
#2800 = FACE_OUTER_BOUND ( 'NONE', #2881, .T. ) ;
#2801 = ORIENTED_EDGE ( 'NONE', *, *, #4183, .T. ) ;
#2802 = CARTESIAN_POINT ( 'NONE',  ( -50.79490495164537833, -30.00000000000000355, -82.50000000000001421 ) ) ;
#2803 = ORIENTED_EDGE ( 'NONE', *, *, #3833, .F. ) ;
#2804 = DIRECTION ( 'NONE',  ( -0.000000000000000000, -0.000000000000000000, -1.000000000000000000 ) ) ;
#2805 = VECTOR ( 'NONE', #2421, 1000.000000000000000 ) ;
#2806 = FACE_OUTER_BOUND ( 'NONE', #266, .T. ) ;
#2807 = EDGE_CURVE ( 'NONE', #4540, #95, #5755, .T. ) ;
#2808 = DIRECTION ( 'NONE',  ( -1.000000000000000000, 0.000000000000000000, 0.000000000000000000 ) ) ;
#2809 = CARTESIAN_POINT ( 'NONE',  ( 19.50000000000000355, 2.356749903719115078E-13, 5.000000000000000000 ) ) ;
#2810 = EDGE_CURVE ( 'NONE', #3864, #2503, #6978, .T. ) ;
#2811 = CARTESIAN_POINT ( 'NONE',  ( -1.463718181065716051, -28.32253049495585273, 1.359567973934762142 ) ) ;
#2812 = EDGE_LOOP ( 'NONE', ( #7167, #136, #1893, #3376 ) ) ;
#2813 = CIRCLE ( 'NONE', #2967, 6.000000000000000888 ) ;
#2814 = ORIENTED_EDGE ( 'NONE', *, *, #7466, .F. ) ;
#2815 = DIRECTION ( 'NONE',  ( -1.000000000000000000, 0.000000000000000000, 0.000000000000000000 ) ) ;
#2816 = ORIENTED_EDGE ( 'NONE', *, *, #3657, .T. ) ;
#2817 = CARTESIAN_POINT ( 'NONE',  ( 0.000000000000000000, 0.000000000000000000, 20.00000000000000000 ) ) ;
#2818 = DIRECTION ( 'NONE',  ( 0.000000000000000000, 0.000000000000000000, -1.000000000000000000 ) ) ;
#2819 = CIRCLE ( 'NONE', #2049, 26.99999999999999645 ) ;
#2820 = DIRECTION ( 'NONE',  ( -1.000000000000000000, 0.000000000000000000, 0.000000000000000000 ) ) ;
#2821 = CARTESIAN_POINT ( 'NONE',  ( -30.99999999999996803, 2.143131898507869037E-15, 49.50000000000000000 ) ) ;
#2822 = VECTOR ( 'NONE', #7718, 1000.000000000000000 ) ;
#2823 = EDGE_CURVE ( 'NONE', #5944, #3926, #6201, .T. ) ;
#2824 = LINE ( 'NONE', #4268, #9111 ) ;
#2825 = FACE_OUTER_BOUND ( 'NONE', #1220, .T. ) ;
#2826 = VERTEX_POINT ( 'NONE', #9112 ) ;
#2827 = ORIENTED_EDGE ( 'NONE', *, *, #8231, .F. ) ;
#2828 = CARTESIAN_POINT ( 'NONE',  ( 5.000000000000000000, -7.653668647301985040, 18.47759065022880520 ) ) ;
#2829 = FACE_OUTER_BOUND ( 'NONE', #7753, .T. ) ;
#2830 = ADVANCED_FACE ( 'NONE', ( #8305, #4659, #7582, #4755, #998 ), #4033, .T. ) ;
#2831 = VECTOR ( 'NONE', #6778, 1000.000000000000000 ) ;
#2832 = ADVANCED_FACE ( 'NONE', ( #2501 ), #5428, .T. ) ;
#2833 = AXIS2_PLACEMENT_3D ( 'NONE', #1756, #2488, #3245 ) ;
#2834 = CARTESIAN_POINT ( 'NONE',  ( 0.000000000000000000, 0.000000000000000000, 0.000000000000000000 ) ) ;
#2835 = ADVANCED_FACE ( 'NONE', ( #5474 ), #8959, .T. ) ;
#2836 = EDGE_CURVE ( 'NONE', #3553, #5088, #2824, .T. ) ;
#2837 = DIRECTION ( 'NONE',  ( -0.7071067811865500152, 8.659560562354903276E-17, -0.7071067811865451302 ) ) ;
#2838 = ORIENTED_EDGE ( 'NONE', *, *, #5772, .F. ) ;
#2839 = ORIENTED_EDGE ( 'NONE', *, *, #8643, .F. ) ;
#2840 = ORIENTED_EDGE ( 'NONE', *, *, #3633, .F. ) ;
#2841 = EDGE_LOOP ( 'NONE', ( #4779, #4446, #2513, #6225 ) ) ;
#2842 = CARTESIAN_POINT ( 'NONE',  ( -19.50000000000000000, -7.819093608422630136E-14, 15.00000000000000000 ) ) ;
#2843 = CARTESIAN_POINT ( 'NONE',  ( -6.000000000000000888, 22.50000000000000355, 5.000000000000000000 ) ) ;
#2844 = LINE ( 'NONE', #2662, #9179 ) ;
#2845 = AXIS2_PLACEMENT_3D ( 'NONE', #7721, #1131, #7619 ) ;
#2846 = EDGE_CURVE ( 'NONE', #5930, #5682, #7774, .T. ) ;
#2847 = DIRECTION ( 'NONE',  ( -0.000000000000000000, 1.000000000000000000, 0.000000000000000000 ) ) ;
#2848 = EDGE_CURVE ( 'NONE', #2860, #3262, #2528, .T. ) ;
#2849 = CARTESIAN_POINT ( 'NONE',  ( 27.00000000000000355, -29.99999999999999289, 64.00000000000000000 ) ) ;
#2850 = EDGE_CURVE ( 'NONE', #8610, #5692, #8656, .T. ) ;
#2851 = VERTEX_POINT ( 'NONE', #468 ) ;
#2852 = CARTESIAN_POINT ( 'NONE',  ( 20.14434505884620918, 53.53579249963522102, -2.801156583491397623 ) ) ;
#2853 = ORIENTED_EDGE ( 'NONE', *, *, #7954, .T. ) ;
#2854 = CARTESIAN_POINT ( 'NONE',  ( -6.000000000000000888, -22.50000000000000355, 5.000000000000000000 ) ) ;
#2855 = DIRECTION ( 'NONE',  ( 0.000000000000000000, 0.000000000000000000, 1.000000000000000000 ) ) ;
#2856 = DIRECTION ( 'NONE',  ( -0.7071067811865486830, 0.000000000000000000, -0.7071067811865464625 ) ) ;
#2857 = CARTESIAN_POINT ( 'NONE',  ( 43.18827341296426425, 42.33902489539482872, -7.653089211995569130 ) ) ;
#2858 = AXIS2_PLACEMENT_3D ( 'NONE', #7587, #1910, #6828 ) ;
#2859 = CARTESIAN_POINT ( 'NONE',  ( 1.072052546109581117, -28.40723195920986655, 1.426690145881926552 ) ) ;
#2860 = VERTEX_POINT ( 'NONE', #4077 ) ;
#2861 = ORIENTED_EDGE ( 'NONE', *, *, #2544, .T. ) ;
#2862 = EDGE_LOOP ( 'NONE', ( #5189, #7200, #4391, #3191 ) ) ;
#2863 = CARTESIAN_POINT ( 'NONE',  ( -27.81412668510618502, -2.815004828058397468, 0.9535900900804862301 ) ) ;
#2864 = CARTESIAN_POINT ( 'NONE',  ( 32.00000000000000711, 0.000000000000000000, 32.00000000000000000 ) ) ;
#2865 = CYLINDRICAL_SURFACE ( 'NONE', #1472, 3.000000000000002665 ) ;
#2866 = CIRCLE ( 'NONE', #7457, 6.000000000000001776 ) ;
#2867 = CARTESIAN_POINT ( 'NONE',  ( 27.00000000000000355, 0.000000000000000000, 64.00000000000000000 ) ) ;
#2868 = CARTESIAN_POINT ( 'NONE',  ( -12.37436867076458036, -12.37436867076458036, 19.62563132923542142 ) ) ;
#2869 = DIRECTION ( 'NONE',  ( -0.000000000000000000, -0.000000000000000000, -1.000000000000000000 ) ) ;
#2870 = VECTOR ( 'NONE', #2900, 1000.000000000000114 ) ;
#2871 = ORIENTED_EDGE ( 'NONE', *, *, #2306, .F. ) ;
#2872 = ORIENTED_EDGE ( 'NONE', *, *, #343, .T. ) ;
#2873 = VECTOR ( 'NONE', #6745, 1000.000000000000000 ) ;
#2874 = CARTESIAN_POINT ( 'NONE',  ( 53.29490495164537833, 27.56180520566613268, -41.61356529332876875 ) ) ;
#2875 = AXIS2_PLACEMENT_3D ( 'NONE', #623, #5768, #4944 ) ;
#2876 = VECTOR ( 'NONE', #2150, 1000.000000000000000 ) ;
#2877 = AXIS2_PLACEMENT_3D ( 'NONE', #4144, #6403, #486 ) ;
#2878 = AXIS2_PLACEMENT_3D ( 'NONE', #4076, #3212, #6960 ) ;
#2879 = DIRECTION ( 'NONE',  ( 0.000000000000000000, -0.7071067811865472397, -0.7071067811865479058 ) ) ;
#2880 = CARTESIAN_POINT ( 'NONE',  ( 0.000000000000000000, 14.14213562373112154, -15.70213562373078098 ) ) ;
#2881 = EDGE_LOOP ( 'NONE', ( #2383, #217, #2541, #459 ) ) ;
#2882 = EDGE_LOOP ( 'NONE', ( #793, #4613, #3052, #4181, #354 ) ) ;
#2883 = ORIENTED_EDGE ( 'NONE', *, *, #5481, .T. ) ;
#2884 = VERTEX_POINT ( 'NONE', #4978 ) ;
#2885 = EDGE_CURVE ( 'NONE', #4565, #602, #5593, .T. ) ;
#2886 = DIRECTION ( 'NONE',  ( 0.000000000000000000, 0.000000000000000000, 1.000000000000000000 ) ) ;
#2887 = VECTOR ( 'NONE', #2508, 999.9999999999998863 ) ;
#2888 = EDGE_CURVE ( 'NONE', #7697, #7845, #7821, .T. ) ;
#2889 = CYLINDRICAL_SURFACE ( 'NONE', #3188, 11.00000000000000711 ) ;
#2890 = DIRECTION ( 'NONE',  ( -1.000000000000000000, -0.000000000000000000, -0.000000000000000000 ) ) ;
#2891 = CARTESIAN_POINT ( 'NONE',  ( 0.000000000000000000, 0.000000000000000000, 0.000000000000000000 ) ) ;
#2892 = CARTESIAN_POINT ( 'NONE',  ( 53.29490495164537833, -48.67545040036925030, -60.28901569369804037 ) ) ;
#2893 = FACE_OUTER_BOUND ( 'NONE', #7695, .T. ) ;
#2894 = CIRCLE ( 'NONE', #6436, 1.560000000001466436 ) ;
#2895 = VERTEX_POINT ( 'NONE', #9351 ) ;
#2896 = VECTOR ( 'NONE', #2890, 1000.000000000000000 ) ;
#2897 = CARTESIAN_POINT ( 'NONE',  ( -12.37436867076458036, 12.37436867076458036, 19.62563132923542142 ) ) ;
#2898 = ORIENTED_EDGE ( 'NONE', *, *, #8911, .T. ) ;
#2899 = FACE_OUTER_BOUND ( 'NONE', #7412, .T. ) ;
#2900 = DIRECTION ( 'NONE',  ( -0.5773502691896249539, 0.5773502691896263972, -0.5773502691896258421 ) ) ;
#2901 = EDGE_CURVE ( 'NONE', #1107, #4182, #6820, .T. ) ;
#2902 = CIRCLE ( 'NONE', #9185, 17.50000000000000000 ) ;
#2903 = DIRECTION ( 'NONE',  ( 1.000000000000000000, -0.000000000000000000, -0.000000000000000000 ) ) ;
#2904 = DIRECTION ( 'NONE',  ( -1.000000000000000000, 0.000000000000000000, 0.000000000000000000 ) ) ;
#2905 = VERTEX_POINT ( 'NONE', #5619 ) ;
#2906 = ORIENTED_EDGE ( 'NONE', *, *, #2766, .T. ) ;
#2907 = PRESENTATION_STYLE_ASSIGNMENT (( #4304 ) ) ;
#2908 = VERTEX_POINT ( 'NONE', #1866 ) ;
#2909 = DIRECTION ( 'NONE',  ( 1.000000000000000000, 0.000000000000000000, 0.000000000000000000 ) ) ;
#2910 = FACE_OUTER_BOUND ( 'NONE', #3235, .T. ) ;
#2911 = CARTESIAN_POINT ( 'NONE',  ( -39.50000000000000711, -30.00000000000000355, -82.50000000000001421 ) ) ;
#2912 = DIRECTION ( 'NONE',  ( -1.000000000000000000, 0.000000000000000000, 0.000000000000000000 ) ) ;
#2913 = CARTESIAN_POINT ( 'NONE',  ( 3.500000000000000444, -6.505213034913026604E-16, 1.500000000000000000 ) ) ;
#2914 = DIRECTION ( 'NONE',  ( -1.000000000000000000, 0.000000000000000000, 0.000000000000000000 ) ) ;
#2915 = VERTEX_POINT ( 'NONE', #4796 ) ;
#2916 = VERTEX_POINT ( 'NONE', #1141 ) ;
#2917 = DIRECTION ( 'NONE',  ( -1.000000000000000000, 0.000000000000000000, 0.000000000000000000 ) ) ;
#2918 = DIRECTION ( 'NONE',  ( 0.000000000000000000, 0.000000000000000000, -1.000000000000000000 ) ) ;
#2919 = EDGE_CURVE ( 'NONE', #4339, #6427, #7056, .T. ) ;
#2920 = LINE ( 'NONE', #6005, #6054 ) ;
#2921 = LINE ( 'NONE', #4323, #2423 ) ;
#2922 = ORIENTED_EDGE ( 'NONE', *, *, #1576, .F. ) ;
#2923 = EDGE_CURVE ( 'NONE', #9426, #955, #2060, .T. ) ;
#2924 = VERTEX_POINT ( 'NONE', #4169 ) ;
#2925 = ORIENTED_EDGE ( 'NONE', *, *, #112, .F. ) ;
#2926 = CARTESIAN_POINT ( 'NONE',  ( 7.219041098787931432, 17.17621444547007670, 45.46043998484430659 ) ) ;
#2927 = CIRCLE ( 'NONE', #8304, 7.250000000000002665 ) ;
#2928 = ORIENTED_EDGE ( 'NONE', *, *, #4131, .F. ) ;
#2929 = DIRECTION ( 'NONE',  ( 0.000000000000000000, 0.000000000000000000, -1.000000000000000000 ) ) ;
#2930 = CARTESIAN_POINT ( 'NONE',  ( 22.50000000000000355, 0.000000000000000000, 5.000000000000000000 ) ) ;
#2931 = DIRECTION ( 'NONE',  ( -1.000000000000000000, -0.000000000000000000, -0.000000000000000000 ) ) ;
#2932 = DIRECTION ( 'NONE',  ( 0.7071067811865439090, 0.000000000000000000, -0.7071067811865512365 ) ) ;
#2933 = CARTESIAN_POINT ( 'NONE',  ( -37.00000000000000000, -8.017766952966344007, -116.9822330470336453 ) ) ;
#2934 = FACE_OUTER_BOUND ( 'NONE', #5212, .T. ) ;
#2935 = ORIENTED_EDGE ( 'NONE', *, *, #192, .T. ) ;
#2936 = VERTEX_POINT ( 'NONE', #7094 ) ;
#2937 = VECTOR ( 'NONE', #4298, 1000.000000000000114 ) ;
#2938 = CARTESIAN_POINT ( 'NONE',  ( 0.000000000000000000, 0.000000000000000000, 0.000000000000000000 ) ) ;
#2939 = PRODUCT_DEFINITION ( 'UNKNOWN', '', #9276, #853 ) ;
#2940 = CARTESIAN_POINT ( 'NONE',  ( 2.000000000000000000, 0.000000000000000000, 15.66147716702868209 ) ) ;
#2941 = EDGE_CURVE ( 'NONE', #4363, #7585, #7866, .T. ) ;
#2943 = ADVANCED_FACE ( 'NONE', ( #5761 ), #2779, .F. ) ;
#2942 = CYLINDRICAL_SURFACE ( 'NONE', #1515, 17.50000000000000355 ) ;
#2944 = EDGE_CURVE ( 'NONE', #6191, #651, #420, .T. ) ;
#2945 = DIRECTION ( 'NONE',  ( 0.000000000000000000, 0.000000000000000000, 1.000000000000000000 ) ) ;
#2946 = ADVANCED_FACE ( 'NONE', ( #6299 ), #4889, .F. ) ;
#2947 = VERTEX_POINT ( 'NONE', #6386 ) ;
#2948 = ORIENTED_EDGE ( 'NONE', *, *, #8637, .F. ) ;
#2949 = DIRECTION ( 'NONE',  ( -1.000000000000000000, 0.000000000000000000, 0.000000000000000000 ) ) ;
#2950 = AXIS2_PLACEMENT_3D ( 'NONE', #9180, #2700, #7745 ) ;
#2951 = ORIENTED_EDGE ( 'NONE', *, *, #8563, .T. ) ;
#2952 = DIRECTION ( 'NONE',  ( 0.000000000000000000, 0.000000000000000000, -1.000000000000000000 ) ) ;
#2953 = LINE ( 'NONE', #4542, #2593 ) ;
#2954 = DIRECTION ( 'NONE',  ( -1.000000000000000000, 0.000000000000000000, 0.000000000000000000 ) ) ;
#2955 =( REPRESENTATION_RELATIONSHIP ('NONE','NONE', #1933, #8501 ) REPRESENTATION_RELATIONSHIP_WITH_TRANSFORMATION ( #7828 )SHAPE_REPRESENTATION_RELATIONSHIP( ) );
#2956 = PLANE ( 'NONE',  #5538 ) ;
#2958 = CARTESIAN_POINT ( 'NONE',  ( 0.000000000000000000, 0.000000000000000000, 64.00000000000000000 ) ) ;
#2957 = AXIS2_PLACEMENT_3D ( 'NONE', #6087, #6185, #7563 ) ;
#2959 = EDGE_CURVE ( 'NONE', #5812, #703, #7887, .T. ) ;
#2960 = DIRECTION ( 'NONE',  ( 0.000000000000000000, 0.000000000000000000, -1.000000000000000000 ) ) ;
#2961 = CARTESIAN_POINT ( 'NONE',  ( 0.000000000000000000, 22.50000000000000355, 5.000000000000000000 ) ) ;
#2962 = ORIENTED_EDGE ( 'NONE', *, *, #6156, .T. ) ;
#2963 = ORIENTED_EDGE ( 'NONE', *, *, #5662, .T. ) ;
#2964 = EDGE_CURVE ( 'NONE', #152, #450, #8586, .T. ) ;
#2965 = CARTESIAN_POINT ( 'NONE',  ( -37.00000000000000711, -1.836970198721028011E-15, -85.00000000000000000 ) ) ;
#2966 = CARTESIAN_POINT ( 'NONE',  ( 5.000000000000000000, 9.603694566548697359E-13, 21.56000000000303984 ) ) ;
#2967 = AXIS2_PLACEMENT_3D ( 'NONE', #2415, #252, #966 ) ;
#2968 = CARTESIAN_POINT ( 'NONE',  ( 60.00000000000000000, -15.90990257669733943, -85.90990257669729147 ) ) ;
#2969 = CARTESIAN_POINT ( 'NONE',  ( 37.73845885098648267, -45.76160744848121453, -6.169970105658134862 ) ) ;
#2970 = DIRECTION ( 'NONE',  ( -1.000000000000000000, 0.000000000000000000, 0.000000000000000000 ) ) ;
#2971 = ORIENTED_EDGE ( 'NONE', *, *, #4754, .T. ) ;
#2972 = EDGE_LOOP ( 'NONE', ( #7131, #2609 ) ) ;
#2973 = CARTESIAN_POINT ( 'NONE',  ( 23.57597564296115422, 144.0974543633810185, 57.89746219150362094 ) ) ;
#2974 = ORIENTED_EDGE ( 'NONE', *, *, #6168, .F. ) ;
#2975 = AXIS2_PLACEMENT_3D ( 'NONE', #4464, #5810, #3739 ) ;
#2976 = FACE_OUTER_BOUND ( 'NONE', #3768, .T. ) ;
#2977 = DIRECTION ( 'NONE',  ( 0.000000000000000000, 0.000000000000000000, -1.000000000000000000 ) ) ;
#2978 = AXIS2_PLACEMENT_3D ( 'NONE', #5220, #4599, #8961 ) ;
#2979 = DIRECTION ( 'NONE',  ( 1.000000000000000000, 0.000000000000000000, 0.000000000000000000 ) ) ;
#2980 = DIRECTION ( 'NONE',  ( 0.000000000000000000, 0.000000000000000000, 1.000000000000000000 ) ) ;
#2981 = DIRECTION ( 'NONE',  ( -1.000000000000000000, -0.000000000000000000, -0.000000000000000000 ) ) ;
#2982 = AXIS2_PLACEMENT_3D ( 'NONE', #658, #5171, #8730 ) ;
#2983 = CARTESIAN_POINT ( 'NONE',  ( 2.143131898507868248E-15, 17.50000000000000000, 14.49999999999999822 ) ) ;
#2984 = ORIENTED_EDGE ( 'NONE', *, *, #7963, .F. ) ;
#2985 = DIRECTION ( 'NONE',  ( -1.000000000000000000, 0.000000000000000000, -0.000000000000000000 ) ) ;
#2986 = AXIS2_PLACEMENT_3D ( 'NONE', #3311, #8216, #6206 ) ;
#2987 = VERTEX_POINT ( 'NONE', #2054 ) ;
#2988 = FACE_OUTER_BOUND ( 'NONE', #6451, .T. ) ;
#2989 = DIRECTION ( 'NONE',  ( -1.000000000000000000, 0.000000000000000000, 0.000000000000000000 ) ) ;
#2990 = CARTESIAN_POINT ( 'NONE',  ( -60.00000000000000000, -60.00000000000000000, 0.000000000000000000 ) ) ;
#2991 = DIRECTION ( 'NONE',  ( 0.000000000000000000, 1.000000000000000000, 0.000000000000000000 ) ) ;
#2992 = ORIENTED_EDGE ( 'NONE', *, *, #5521, .T. ) ;
#2993 = AXIS2_PLACEMENT_3D ( 'NONE', #6365, #4372, #2763 ) ;
#2994 = ORIENTED_EDGE ( 'NONE', *, *, #441, .F. ) ;
#2995 =( NAMED_UNIT ( * ) PLANE_ANGLE_UNIT ( ) SI_UNIT ( $, .RADIAN. ) );
#2996 = ORIENTED_EDGE ( 'NONE', *, *, #1589, .T. ) ;
#2997 = CARTESIAN_POINT ( 'NONE',  ( -60.00000000000001421, 9.637301612213114765, -29.99999999999998934 ) ) ;
#2998 = EDGE_CURVE ( 'NONE', #2936, #5896, #5863, .T. ) ;
#2999 = CARTESIAN_POINT ( 'NONE',  ( -9.048619709455110183, 15.70011763207404876, 16.29988236792595657 ) ) ;
#3000 = FACE_BOUND ( 'NONE', #4708, .T. ) ;
#3001 = ADVANCED_FACE ( 'NONE', ( #43 ), #5894, .T. ) ;
#3002 = EDGE_CURVE ( 'NONE', #5323, #8143, #6061, .T. ) ;
#3003 = EDGE_CURVE ( 'NONE', #95, #4540, #1760, .T. ) ;
#3004 = FACE_BOUND ( 'NONE', #5763, .T. ) ;
#3005 = AXIS2_PLACEMENT_3D ( 'NONE', #7298, #5775, #1487 ) ;
#3006 = CARTESIAN_POINT ( 'NONE',  ( -4.703319286132084720, -17.49999999999999645, 14.50000000000000178 ) ) ;
#3007 = DIRECTION ( 'NONE',  ( -1.000000000000000000, 1.224646799147353454E-16, 0.000000000000000000 ) ) ;
#3008 = CARTESIAN_POINT ( 'NONE',  ( -31.99999999999999289, -29.99999999999996447, 0.000000000000000000 ) ) ;
#3009 = ORIENTED_EDGE ( 'NONE', *, *, #5368, .T. ) ;
#3010 = ORIENTED_EDGE ( 'NONE', *, *, #4400, .T. ) ;
#3011 = VECTOR ( 'NONE', #6369, 1000.000000000000000 ) ;
#3012 = CYLINDRICAL_SURFACE ( 'NONE', #4255, 7.250000000000002665 ) ;
#3013 = ORIENTED_EDGE ( 'NONE', *, *, #5966, .F. ) ;
#3014 = DIRECTION ( 'NONE',  ( -0.000000000000000000, -0.000000000000000000, -1.000000000000000000 ) ) ;
#3015 = EDGE_CURVE ( 'NONE', #7382, #2622, #3907, .T. ) ;
#3016 = AXIS2_PLACEMENT_3D ( 'NONE', #213, #4772, #1019 ) ;
#3017 = DIRECTION ( 'NONE',  ( 0.000000000000000000, 0.000000000000000000, -1.000000000000000000 ) ) ;
#3018 = DIRECTION ( 'NONE',  ( 0.000000000000000000, 0.000000000000000000, -1.000000000000000000 ) ) ;
#3019 = TOROIDAL_SURFACE ( 'NONE', #5494, 13.50000000000000178, 1.000000000000000000 ) ;
#3020 = VERTEX_POINT ( 'NONE', #2094 ) ;
#3021 = ORIENTED_EDGE ( 'NONE', *, *, #1957, .T. ) ;
#3022 = CIRCLE ( 'NONE', #8552, 17.50000000000000000 ) ;
#3023 = PRODUCT_CONTEXT ( 'NONE', #1792, 'mechanical' ) ;
#3024 = EDGE_CURVE ( 'NONE', #4140, #424, #7743, .T. ) ;
#3025 = CIRCLE ( 'NONE', #7022, 13.50000000000000178 ) ;
#3026 = AXIS2_PLACEMENT_3D ( 'NONE', #583, #7794, #4951 ) ;
#3027 = CARTESIAN_POINT ( 'NONE',  ( -27.00000000000000000, 43.00000000000000000, 11.99999999999999645 ) ) ;
#3028 =( BOUNDED_CURVE ( )  B_SPLINE_CURVE ( 3, ( #3567, #685, #2130, #6506 ),
 .UNSPECIFIED., .F., .F. ) 
 B_SPLINE_CURVE_WITH_KNOTS ( ( 4, 4 ),
 ( 4.712388980384689674, 7.853981633974482790 ),
 .UNSPECIFIED. ) 
 CURVE ( )  GEOMETRIC_REPRESENTATION_ITEM ( )  RATIONAL_B_SPLINE_CURVE ( ( 1.000000000000000000, 0.3333333333333333703, 0.3333333333333333703, 1.000000000000000000 ) ) 
 REPRESENTATION_ITEM ( '' )  );
#3029 = DIRECTION ( 'NONE',  ( -1.000000000000000000, 0.000000000000000000, 0.000000000000000000 ) ) ;
#3030 = VECTOR ( 'NONE', #1334, 1000.000000000000000 ) ;
#3031 = DIRECTION ( 'NONE',  ( -0.000000000000000000, -0.000000000000000000, -1.000000000000000000 ) ) ;
#3032 = AXIS2_PLACEMENT_3D ( 'NONE', #1468, #3636, #5895 ) ;
#3033 = CARTESIAN_POINT ( 'NONE',  ( 5.000000000000000000, 14.14213562373247868, 12.58213562373372341 ) ) ;
#3034 = CARTESIAN_POINT ( 'NONE',  ( -12.37436867076458036, 12.37436867076458036, 19.62563132923542142 ) ) ;
#3035 = CIRCLE ( 'NONE', #5499, 17.50000000000000355 ) ;
#3036 = DIRECTION ( 'NONE',  ( 0.000000000000000000, 0.000000000000000000, -1.000000000000000000 ) ) ;
#3037 = EDGE_LOOP ( 'NONE', ( #6137, #5186, #3668, #1761 ) ) ;
#3038 =( LENGTH_UNIT ( ) NAMED_UNIT ( * ) SI_UNIT ( .MILLI., .METRE. ) );
#3039 = CIRCLE ( 'NONE', #130, 18.50000000000000355 ) ;
#3040 = VERTEX_POINT ( 'NONE', #6717 ) ;
#3041 = DIRECTION ( 'NONE',  ( -1.000000000000000000, 0.000000000000000000, 0.000000000000000000 ) ) ;
#3042 = CARTESIAN_POINT ( 'NONE',  ( -32.83333333333333570, -21.66666666666668206, -90.83333333333332860 ) ) ;
#3043 = DIRECTION ( 'NONE',  ( -0.000000000000000000, -0.000000000000000000, 1.000000000000000000 ) ) ;
#3044 = EDGE_CURVE ( 'NONE', #5200, #754, #5288, .T. ) ;
#3045 = VECTOR ( 'NONE', #1030, 1000.000000000000000 ) ;
#3046 = LINE ( 'NONE', #3142, #8160 ) ;
#3047 = CIRCLE ( 'NONE', #4890, 5.000000000000000888 ) ;
#3048 = CIRCLE ( 'NONE', #7675, 26.99999999999997868 ) ;
#3049 = ORIENTED_EDGE ( 'NONE', *, *, #7347, .T. ) ;
#3050 = ORIENTED_EDGE ( 'NONE', *, *, #7174, .T. ) ;
#3051 = EDGE_CURVE ( 'NONE', #85, #3983, #7586, .T. ) ;
#3052 = ORIENTED_EDGE ( 'NONE', *, *, #1961, .T. ) ;
#3053 = CARTESIAN_POINT ( 'NONE',  ( 2.060470863510026174, 28.13894063079881391, 1.213559982043999952 ) ) ;
#3054 = EDGE_LOOP ( 'NONE', ( #4141, #4486, #1243, #4327 ) ) ;
#3055 = CYLINDRICAL_SURFACE ( 'NONE', #8726, 3.000000000000002665 ) ;
#3056 = DIRECTION ( 'NONE',  ( -1.000000000000000000, 0.000000000000000000, 0.000000000000000000 ) ) ;
#3057 = AXIS2_PLACEMENT_3D ( 'NONE', #3851, #6068, #3998 ) ;
#3058 = DIRECTION ( 'NONE',  ( -0.000000000000000000, -0.000000000000000000, -1.000000000000000000 ) ) ;
#3059 = AXIS2_PLACEMENT_3D ( 'NONE', #6844, #4005, #4813 ) ;
#3060 = CARTESIAN_POINT ( 'NONE',  ( 0.000000000000000000, 35.00000000000000000, 32.00000000000000000 ) ) ;
#3061 = CARTESIAN_POINT ( 'NONE',  ( 14.49999999999998401, 1.806354028742345013E-15, 27.50000000000000355 ) ) ;
#3062 = CARTESIAN_POINT ( 'NONE',  ( 0.000000000000000000, 0.000000000000000000, 0.000000000000000000 ) ) ;
#3063 = CYLINDRICAL_SURFACE ( 'NONE', #1586, 6.000000000000000888 ) ;
#3064 = ORIENTED_EDGE ( 'NONE', *, *, #1007, .T. ) ;
#3065 = EDGE_LOOP ( 'NONE', ( #615, #3463, #6505, #3674 ) ) ;
#3066 = DIRECTION ( 'NONE',  ( 0.000000000000000000, 0.000000000000000000, 1.000000000000000000 ) ) ;
#3067 = ORIENTED_EDGE ( 'NONE', *, *, #8813, .F. ) ;
#3068 = DIRECTION ( 'NONE',  ( -0.000000000000000000, -0.000000000000000000, 1.000000000000000000 ) ) ;
#3069 = EDGE_CURVE ( 'NONE', #3097, #8797, #7330, .T. ) ;
#3070 = AXIS2_PLACEMENT_3D ( 'NONE', #2211, #2979, #863 ) ;
#3071 = EDGE_CURVE ( 'NONE', #703, #5812, #988, .T. ) ;
#3072 = CARTESIAN_POINT ( 'NONE',  ( 0.000000000000000000, -34.99999999999999289, 32.00000000000000000 ) ) ;
#3073 = UNCERTAINTY_MEASURE_WITH_UNIT (LENGTH_MEASURE( 1.000000000000000082E-05 ), #6901, 'distance_accuracy_value', 'NONE');
#3074 = CARTESIAN_POINT ( 'NONE',  ( -1.749999999999984235, 1.750000000000001554, 0.000000000000000000 ) ) ;
#3075 = ORIENTED_EDGE ( 'NONE', *, *, #2371, .F. ) ;
#3076 = ORIENTED_EDGE ( 'NONE', *, *, #2433, .F. ) ;
#3077 = DIRECTION ( 'NONE',  ( 0.000000000000000000, 0.000000000000000000, 1.000000000000000000 ) ) ;
#3078 = CARTESIAN_POINT ( 'NONE',  ( 0.000000000000000000, 22.50000000000000355, 5.000000000000000000 ) ) ;
#3079 = AXIS2_PLACEMENT_3D ( 'NONE', #5119, #6573, #9394 ) ;
#3080 = DIRECTION ( 'NONE',  ( 1.000000000000000000, 0.000000000000000000, 0.000000000000000000 ) ) ;
#3081 = DIRECTION ( 'NONE',  ( 0.000000000000000000, 0.000000000000000000, 1.000000000000000000 ) ) ;
#3082 = DIRECTION ( 'NONE',  ( -0.7071067811865494601, -0.4999999999999988343, 0.4999999999999985012 ) ) ;
#3083 = FACE_OUTER_BOUND ( 'NONE', #3263, .T. ) ;
#3084 = VECTOR ( 'NONE', #4690, 1000.000000000000000 ) ;
#3085 = ORIENTED_EDGE ( 'NONE', *, *, #4357, .T. ) ;
#3086 = DIRECTION ( 'NONE',  ( 0.000000000000000000, -0.7071067811865451302, -0.7071067811865500152 ) ) ;
#3087 = EDGE_LOOP ( 'NONE', ( #8205, #8824, #6605, #1657 ) ) ;
#3088 = CARTESIAN_POINT ( 'NONE',  ( -53.29490495164537833, -30.00000000000000000, -41.61356529332876875 ) ) ;
#3089 = LINE ( 'NONE', #3042, #2870 ) ;
#3090 = DIRECTION ( 'NONE',  ( 0.000000000000000000, 1.000000000000000000, 0.000000000000000000 ) ) ;
#3091 = CARTESIAN_POINT ( 'NONE',  ( 0.000000000000000000, -22.50000000000000355, 0.000000000000000000 ) ) ;
#3092 = VERTEX_POINT ( 'NONE', #3776 ) ;
#3093 = AXIS2_PLACEMENT_3D ( 'NONE', #7315, #5207, #1654 ) ;
#3094 = ORIENTED_EDGE ( 'NONE', *, *, #8986, .T. ) ;
#3095 = EDGE_LOOP ( 'NONE', ( #256, #8733, #2962, #7986 ) ) ;
#3096 =( NAMED_UNIT ( * ) SI_UNIT ( $, .STERADIAN. ) SOLID_ANGLE_UNIT ( ) );
#3097 = VERTEX_POINT ( 'NONE', #8679 ) ;
#3098 = CARTESIAN_POINT ( 'NONE',  ( 27.00000000000000000, -43.00000000000000000, 25.00000000000000000 ) ) ;
#3099 = CARTESIAN_POINT ( 'NONE',  ( 22.50000000000000355, 2.356749903719115078E-13, 0.000000000000000000 ) ) ;
#3100 = PLANE ( 'NONE',  #4555 ) ;
#3101 = CIRCLE ( 'NONE', #338, 6.000000000000000888 ) ;
#3102 = DIRECTION ( 'NONE',  ( -1.000000000000000000, 0.000000000000000000, 0.000000000000000000 ) ) ;
#3103 = EDGE_CURVE ( 'NONE', #3697, #794, #7274, .T. ) ;
#3104 = CARTESIAN_POINT ( 'NONE',  ( 19.62310601229374285, 19.62310601229374285, 37.12563132923541787 ) ) ;
#3105 = DIRECTION ( 'NONE',  ( -1.000000000000000000, -0.000000000000000000, -0.000000000000000000 ) ) ;
#3106 = CIRCLE ( 'NONE', #4947, 15.00000000000000000 ) ;
#3107 = DIRECTION ( 'NONE',  ( -1.000000000000000000, 0.000000000000000000, 0.000000000000000000 ) ) ;
#3108 = ORIENTED_EDGE ( 'NONE', *, *, #952, .F. ) ;
#3109 = ORIENTED_EDGE ( 'NONE', *, *, #3426, .F. ) ;
#3110 = DIRECTION ( 'NONE',  ( 1.000000000000000000, 0.000000000000000000, 0.000000000000000000 ) ) ;
#3111 = ORIENTED_EDGE ( 'NONE', *, *, #6, .F. ) ;
#3112 = LINE ( 'NONE', #369, #7410 ) ;
#3113 = ORIENTED_EDGE ( 'NONE', *, *, #5440, .F. ) ;
#3114 = VECTOR ( 'NONE', #4688, 999.9999999999998863 ) ;
#3115 = EDGE_CURVE ( 'NONE', #3433, #7709, #6574, .T. ) ;
#3116 = CARTESIAN_POINT ( 'NONE',  ( 31.00000000000002132, 0.000000000000000000, 14.49999999999999467 ) ) ;
#3117 = CARTESIAN_POINT ( 'NONE',  ( 0.000000000000000000, 0.000000000000000000, 10.00000000000000000 ) ) ;
#3118 = DIRECTION ( 'NONE',  ( -0.000000000000000000, -0.000000000000000000, -1.000000000000000000 ) ) ;
#3119 = ORIENTED_EDGE ( 'NONE', *, *, #6547, .T. ) ;
#3120 = VERTEX_POINT ( 'NONE', #2146 ) ;
#3121 = AXIS2_PLACEMENT_3D ( 'NONE', #1899, #547, #4831 ) ;
#3122 = DIRECTION ( 'NONE',  ( 0.9994148367277967404, 0.0008129226918946344613, 0.03419536935095431746 ) ) ;
#3123 = EDGE_CURVE ( 'NONE', #4316, #3234, #5121, .T. ) ;
#3124 = DIRECTION ( 'NONE',  ( -1.000000000000000000, 0.000000000000000000, 0.000000000000000000 ) ) ;
#3125 = CARTESIAN_POINT ( 'NONE',  ( 0.000000000000000000, 22.50000000000000355, 15.00000000000000000 ) ) ;
#3126 = ADVANCED_FACE ( 'NONE', ( #842 ), #5076, .F. ) ;
#3127 = EDGE_CURVE ( 'NONE', #2334, #3397, #5221, .T. ) ;
#3128 = EDGE_CURVE ( 'NONE', #6362, #8767, #701, .T. ) ;
#3129 = DIRECTION ( 'NONE',  ( -1.000000000000000000, 0.000000000000000000, 0.000000000000000000 ) ) ;
#3130 =( NAMED_UNIT ( * ) PLANE_ANGLE_UNIT ( ) SI_UNIT ( $, .RADIAN. ) );
#3131 = FACE_OUTER_BOUND ( 'NONE', #8282, .T. ) ;
#3132 = CYLINDRICAL_SURFACE ( 'NONE', #4195, 15.00000000000000000 ) ;
#3133 = ORIENTED_EDGE ( 'NONE', *, *, #5299, .F. ) ;
#3134 = AXIS2_PLACEMENT_3D ( 'NONE', #3488, #1272, #6339 ) ;
#3135 = ORIENTED_EDGE ( 'NONE', *, *, #1853, .T. ) ;
#3136 = CARTESIAN_POINT ( 'NONE',  ( -27.00000000000000000, -43.00000000000000000, 11.99999999999999645 ) ) ;
#3137 = B_SPLINE_CURVE_WITH_KNOTS ( 'NONE', 3,
 ( #9023, #3840, #6873, #291, #3214, #2459, #7631, #8208, #4562, #6158, #7487, #3165, #2502, #7539, #2404, #954, #6822, #5386, #5429, #1051, #1142, #9160, #8631, #6387, #4891, #561 ),
 .UNSPECIFIED., .F., .F.,
 ( 4, 2, 2, 2, 2, 2, 2, 2, 2, 2, 2, 2, 4 ),
 ( 1.812491582141323212E-18, 0.002002306497011713607, 0.004004612994023425479, 0.005005766242529281415, 0.006006919491035139086, 0.007008072739540995022, 0.008009225988046852693, 0.01001153248505856456, 0.01101268573356442224, 0.01201383898207027817, 0.01301499223057613411, 0.01401614547908198831, 0.01601845197609370539 ),
 .UNSPECIFIED. ) ;
#3138 = DIRECTION ( 'NONE',  ( -1.000000000000000000, -0.000000000000000000, -0.000000000000000000 ) ) ;
#3139 = EDGE_CURVE ( 'NONE', #4945, #7603, #6827, .T. ) ;
#3140 = EDGE_CURVE ( 'NONE', #7436, #8998, #8153, .T. ) ;
#3141 = AXIS2_PLACEMENT_3D ( 'NONE', #791, #4358, #3732 ) ;
#3142 = CARTESIAN_POINT ( 'NONE',  ( -34.25000000000000000, -43.00000000000000000, -25.00000000000000000 ) ) ;
#3143 = ADVANCED_FACE ( 'NONE', ( #448 ), #7797, .F. ) ;
#3144 = VERTEX_POINT ( 'NONE', #6768 ) ;
#3145 = AXIS2_PLACEMENT_3D ( 'NONE', #4198, #5789, #8616 ) ;
#3146 = ORIENTED_EDGE ( 'NONE', *, *, #894, .F. ) ;
#3147 = ORIENTED_EDGE ( 'NONE', *, *, #8411, .T. ) ;
#3148 = VERTEX_POINT ( 'NONE', #1710 ) ;
#3149 = CARTESIAN_POINT ( 'NONE',  ( 2.143131898507868248E-15, -17.50000000000000000, 14.49999999999999822 ) ) ;
#3150 = DIRECTION ( 'NONE',  ( 0.000000000000000000, 0.000000000000000000, 1.000000000000000000 ) ) ;
#3151 = CARTESIAN_POINT ( 'NONE',  ( 2.143131898507868248E-15, 17.50000000000000000, 14.49999999999999822 ) ) ;
#3152 = DIRECTION ( 'NONE',  ( 0.000000000000000000, 0.000000000000000000, 1.000000000000000000 ) ) ;
#3153 = CYLINDRICAL_SURFACE ( 'NONE', #2745, 6.000000000000001776 ) ;
#3154 = LINE ( 'NONE', #1888, #4366 ) ;
#3155 = DIRECTION ( 'NONE',  ( 0.000000000000000000, 0.000000000000000000, 1.000000000000000000 ) ) ;
#3156 = ORIENTED_EDGE ( 'NONE', *, *, #7323, .F. ) ;
#3157 = ORIENTED_EDGE ( 'NONE', *, *, #6652, .F. ) ;
#3158 = CARTESIAN_POINT ( 'NONE',  ( 60.00000000000000000, 12.50000000000000000, -100.0000000000000000 ) ) ;
#3159 = ORIENTED_EDGE ( 'NONE', *, *, #8922, .F. ) ;
#3160 = FACE_BOUND ( 'NONE', #3555, .T. ) ;
#3161 = ORIENTED_EDGE ( 'NONE', *, *, #9436, .T. ) ;
#3162 = DIRECTION ( 'NONE',  ( 1.000000000000000000, 0.000000000000000000, 0.000000000000000000 ) ) ;
#3163 = EDGE_CURVE ( 'NONE', #651, #9261, #3154, .T. ) ;
#3164 = FACE_OUTER_BOUND ( 'NONE', #1257, .T. ) ;
#3165 = CARTESIAN_POINT ( 'NONE',  ( 0.6837532375831764098, -28.73276100836656610, 1.738917791092793319 ) ) ;
#3166 = VECTOR ( 'NONE', #508, 1000.000000000000000 ) ;
#3167 = ORIENTED_EDGE ( 'NONE', *, *, #7958, .T. ) ;
#3168 = EDGE_LOOP ( 'NONE', ( #4694, #4602, #3113, #9102, #4933, #8928 ) ) ;
#3169 = CARTESIAN_POINT ( 'NONE',  ( -27.00000000000000000, -43.00000000000000000, 11.99999999999999645 ) ) ;
#3170 = CARTESIAN_POINT ( 'NONE',  ( 17.49999999999999645, -4.703319286132084720, 49.50000000000000000 ) ) ;
#3171 = AXIS2_PLACEMENT_3D ( 'NONE', #6186, #9095, #1799 ) ;
#3172 = AXIS2_PLACEMENT_3D ( 'NONE', #5069, #1459, #8766 ) ;
#3173 = CARTESIAN_POINT ( 'NONE',  ( 22.50000000000000355, 2.356749903719115078E-13, 10.00000000000000000 ) ) ;
#3174 = DIRECTION ( 'NONE',  ( 1.000000000000000000, 0.000000000000000000, 0.000000000000000000 ) ) ;
#3175 = DIRECTION ( 'NONE',  ( -0.000000000000000000, -0.000000000000000000, -1.000000000000000000 ) ) ;
#3176 = CARTESIAN_POINT ( 'NONE',  ( -37.00000000000000711, 15.90990257669733943, -88.90990257669730568 ) ) ;
#3177 = CIRCLE ( 'NONE', #9002, 17.50000000000000000 ) ;
#3178 = VERTEX_POINT ( 'NONE', #7751 ) ;
#3179 = ADVANCED_FACE ( 'NONE', ( #2392 ), #3825, .T. ) ;
#3180 = EDGE_CURVE ( 'NONE', #2727, #4405, #9263, .T. ) ;
#3181 = EDGE_LOOP ( 'NONE', ( #7722, #9133, #548, #3109 ) ) ;
#3182 = TOROIDAL_SURFACE ( 'NONE', #4406, 5.000000000000000888, 1.000000000000000000 ) ;
#3183 = DIRECTION ( 'NONE',  ( 1.000000000000000000, 0.000000000000000000, -0.000000000000000000 ) ) ;
#3184 = MANIFOLD_SOLID_BREP ( 'Radyus1', #5479 ) ;
#3185 = CARTESIAN_POINT ( 'NONE',  ( -30.99999999999996803, 0.000000000000000000, 14.49999999999999467 ) ) ;
#3186 = AXIS2_PLACEMENT_3D ( 'NONE', #3756, #6839, #8136 ) ;
#3187 = DIRECTION ( 'NONE',  ( 0.000000000000000000, 0.7071067811865479058, -0.7071067811865472397 ) ) ;
#3188 = AXIS2_PLACEMENT_3D ( 'NONE', #5819, #5912, #2263 ) ;
#3189 = FACE_OUTER_BOUND ( 'NONE', #2226, .T. ) ;
#3190 = ADVANCED_FACE ( 'NONE', ( #1160, #4644 ), #2444, .T. ) ;
#3191 = ORIENTED_EDGE ( 'NONE', *, *, #8118, .T. ) ;
#3192 = VECTOR ( 'NONE', #6914, 1000.000000000000000 ) ;
#3193 = ORIENTED_EDGE ( 'NONE', *, *, #7399, .T. ) ;
#3194 = ORIENTED_EDGE ( 'NONE', *, *, #4124, .T. ) ;
#3195 = ORIENTED_EDGE ( 'NONE', *, *, #1853, .F. ) ;
#3196 = CARTESIAN_POINT ( 'NONE',  ( 0.000000000000000000, -7.653668647303860872, -18.47759065022490432 ) ) ;
#3197 = CARTESIAN_POINT ( 'NONE',  ( -40.05867498135627613, -15.23141075423628799, -98.05867498135629035 ) ) ;
#3198 = DIRECTION ( 'NONE',  ( -0.000000000000000000, -0.000000000000000000, -1.000000000000000000 ) ) ;
#3199 = AXIS2_PLACEMENT_3D ( 'NONE', #5615, #8537, #1958 ) ;
#3200 = DIRECTION ( 'NONE',  ( 0.7071067811865441310, -0.7071067811865510144, -0.000000000000000000 ) ) ;
#3201 = CARTESIAN_POINT ( 'NONE',  ( 28.27439555746435929, 1.684082973785338444, 1.321420441384549838 ) ) ;
#3202 = DIRECTION ( 'NONE',  ( -0.7071067811865456854, 3.969829082701935600E-15, -0.7071067811865493491 ) ) ;
#3203 = DIRECTION ( 'NONE',  ( 0.000000000000000000, 0.000000000000000000, 1.000000000000000000 ) ) ;
#3204 = ORIENTED_EDGE ( 'NONE', *, *, #5960, .T. ) ;
#3205 = ORIENTED_EDGE ( 'NONE', *, *, #8629, .T. ) ;
#3206 = DIRECTION ( 'NONE',  ( -0.7071067811865461294, 0.7071067811865489050, 3.840706726830345682E-15 ) ) ;
#3207 = AXIS2_PLACEMENT_3D ( 'NONE', #2284, #5214, #1562 ) ;
#3208 = ORIENTED_EDGE ( 'NONE', *, *, #7362, .F. ) ;
#3209 = FACE_BOUND ( 'NONE', #3564, .T. ) ;
#3210 = AXIS2_PLACEMENT_3D ( 'NONE', #4529, #4482, #6753 ) ;
#3211 = VERTEX_POINT ( 'NONE', #5321 ) ;
#3212 = DIRECTION ( 'NONE',  ( 0.000000000000000000, 0.000000000000000000, -1.000000000000000000 ) ) ;
#3213 = DIRECTION ( 'NONE',  ( -1.000000000000000000, 0.000000000000000000, 0.000000000000000000 ) ) ;
#3214 = CARTESIAN_POINT ( 'NONE',  ( 4.531045531831497719, -27.74104493317181053, 1.101386028467601141 ) ) ;
#3215 = ORIENTED_EDGE ( 'NONE', *, *, #6649, .T. ) ;
#3216 = VERTEX_POINT ( 'NONE', #5274 ) ;
#3217 = ITEM_DEFINED_TRANSFORMATION ( 'NONE', 'NONE', #2993,  #1614 ) ;
#3218 = EDGE_CURVE ( 'NONE', #8254, #4201, #4600, .T. ) ;
#3219 = ADVANCED_FACE ( 'NONE', ( #4147 ), #5594, .F. ) ;
#3220 = CARTESIAN_POINT ( 'NONE',  ( -22.50000000000000355, 0.000000000000000000, 0.000000000000000000 ) ) ;
#3221 = DIRECTION ( 'NONE',  ( -1.000000000000000000, 0.000000000000000000, 0.000000000000000000 ) ) ;
#3222 = EDGE_CURVE ( 'NONE', #3936, #9261, #5548, .T. ) ;
#3223 = LINE ( 'NONE', #1828, #4479 ) ;
#3224 = LINE ( 'NONE', #6262, #2457 ) ;
#3225 = DIRECTION ( 'NONE',  ( 0.000000000000000000, 0.000000000000000000, 1.000000000000000000 ) ) ;
#3226 = EDGE_LOOP ( 'NONE', ( #3119, #1301, #1255, #8020, #3597, #4445 ) ) ;
#3227 = ORIENTED_EDGE ( 'NONE', *, *, #8571, .F. ) ;
#3228 = DIRECTION ( 'NONE',  ( 0.000000000000000000, 0.000000000000000000, 1.000000000000000000 ) ) ;
#3229 = CARTESIAN_POINT ( 'NONE',  ( 0.000000000000000000, 0.000000000000000000, 0.000000000000000000 ) ) ;
#3230 = EDGE_CURVE ( 'NONE', #7510, #7709, #6858, .T. ) ;
#3231 = DIRECTION ( 'NONE',  ( -0.7071067811865441310, 0.7071067811865507924, -0.000000000000000000 ) ) ;
#3232 = DIRECTION ( 'NONE',  ( -1.000000000000000000, -0.000000000000000000, -0.000000000000000000 ) ) ;
#3233 = AXIS2_PLACEMENT_3D ( 'NONE', #225, #6663, #5271 ) ;
#3234 = VERTEX_POINT ( 'NONE', #6145 ) ;
#3235 = EDGE_LOOP ( 'NONE', ( #6864, #2548, #1313, #1315 ) ) ;
#3236 = VERTEX_POINT ( 'NONE', #2489 ) ;
#3237 = EDGE_LOOP ( 'NONE', ( #1066, #8967, #220, #7178 ) ) ;
#3238 = CARTESIAN_POINT ( 'NONE',  ( 0.4999999999999935052, 0.000000000000000000, 22.50000000000000000 ) ) ;
#3239 = EDGE_CURVE ( 'NONE', #3622, #8690, #8474, .T. ) ;
#3240 = DIRECTION ( 'NONE',  ( 0.000000000000000000, 0.000000000000000000, -1.000000000000000000 ) ) ;
#3241 = ADVANCED_FACE ( 'NONE', ( #536, #3513, #1446, #7844, #5825, #4189, #7115, #5738, #7305, #3418, #4336, #2167, #2030, #5690, #9374, #1252, #5642, #586 ), #2707, .T. ) ;
#3242 = DIRECTION ( 'NONE',  ( -1.000000000000000000, 0.000000000000000000, 0.000000000000000000 ) ) ;
#3243 = ADVANCED_FACE ( 'NONE', ( #8657 ), #6503, .F. ) ;
#3244 = CARTESIAN_POINT ( 'NONE',  ( 51.96152422706632024, 29.99999999999999645, -12.99999999999999822 ) ) ;
#3245 = DIRECTION ( 'NONE',  ( -1.000000000000000000, 0.000000000000000000, 0.000000000000000000 ) ) ;
#3246 = ADVANCED_FACE ( 'NONE', ( #2800 ), #2122, .F. ) ;
#3247 = CIRCLE ( 'NONE', #1556, 22.00000000000000711 ) ;
#3248 = DIRECTION ( 'NONE',  ( 0.000000000000000000, 1.000000000000000000, 0.000000000000000000 ) ) ;
#3249 = ORIENTED_EDGE ( 'NONE', *, *, #7638, .T. ) ;
#3250 = ORIENTED_EDGE ( 'NONE', *, *, #5595, .F. ) ;
#3251 = CARTESIAN_POINT ( 'NONE',  ( 5.000000000000000000, -7.653668647301985040, 19.22759065022772873 ) ) ;
#3252 = ORIENTED_EDGE ( 'NONE', *, *, #4958, .T. ) ;
#3253 = LINE ( 'NONE', #7182, #1352 ) ;
#3254 = ORIENTED_EDGE ( 'NONE', *, *, #9208, .F. ) ;
#3255 = AXIS2_PLACEMENT_3D ( 'NONE', #4377, #3661, #8792 ) ;
#3256 = CARTESIAN_POINT ( 'NONE',  ( 37.22467645238199196, 47.05659850664387278, -5.608807313787652404 ) ) ;
#3257 = EDGE_CURVE ( 'NONE', #6494, #5769, #3788, .T. ) ;
#3258 = EDGE_CURVE ( 'NONE', #7366, #5235, #7165, .T. ) ;
#3259 = CYLINDRICAL_SURFACE ( 'NONE', #4673, 30.00000000000000000 ) ;
#3260 = CARTESIAN_POINT ( 'NONE',  ( 22.50000000000000355, 0.000000000000000000, 2.000000000000035083 ) ) ;
#3261 = ADVANCED_FACE ( 'NONE', ( #6407 ), #4957, .T. ) ;
#3262 = VERTEX_POINT ( 'NONE', #5057 ) ;
#3263 = EDGE_LOOP ( 'NONE', ( #1340, #8260, #4635, #7293 ) ) ;
#3264 = AXIS2_PLACEMENT_3D ( 'NONE', #2326, #6214, #3183 ) ;
#3265 = FACE_OUTER_BOUND ( 'NONE', #2792, .T. ) ;
#3266 =( REPRESENTATION_RELATIONSHIP ('NONE','NONE', #1933, #1625 ) REPRESENTATION_RELATIONSHIP_WITH_TRANSFORMATION ( #6971 )SHAPE_REPRESENTATION_RELATIONSHIP( ) );
#3267 = LINE ( 'NONE', #9032, #6221 ) ;
#3268 = CYLINDRICAL_SURFACE ( 'NONE', #7814, 15.00000000000000000 ) ;
#3269 = AXIS2_PLACEMENT_3D ( 'NONE', #1830, #3225, #5395 ) ;
#3270 = DIRECTION ( 'NONE',  ( -1.000000000000000000, -0.000000000000000000, -0.000000000000000000 ) ) ;
#3271 = ORIENTED_EDGE ( 'NONE', *, *, #5604, .T. ) ;
#3272 = FACE_BOUND ( 'NONE', #503, .T. ) ;
#3273 = AXIS2_PLACEMENT_3D ( 'NONE', #7724, #6814, #6957 ) ;
#3274 = ORIENTED_EDGE ( 'NONE', *, *, #814, .T. ) ;
#3275 = DIRECTION ( 'NONE',  ( 0.000000000000000000, 0.000000000000000000, -1.000000000000000000 ) ) ;
#3276 = DIRECTION ( 'NONE',  ( 0.000000000000000000, 0.000000000000000000, 1.000000000000000000 ) ) ;
#3277 = AXIS2_PLACEMENT_3D ( 'NONE', #1758, #4693, #942 ) ;
#3278 = FACE_OUTER_BOUND ( 'NONE', #5671, .T. ) ;
#3279 =( BOUNDED_CURVE ( )  B_SPLINE_CURVE ( 3, ( #3609, #4861, #6546, #9467 ),
 .UNSPECIFIED., .F., .T. ) 
 B_SPLINE_CURVE_WITH_KNOTS ( ( 4, 4 ),
 ( 3.213317012039607956, 4.712388980384689674 ),
 .UNSPECIFIED. ) 
 CURVE ( )  GEOMETRIC_REPRESENTATION_ITEM ( )  RATIONAL_B_SPLINE_CURVE ( ( 1.000000000000000000, 0.8213367208436770373, 0.8213367208436770373, 1.000000000000000000 ) ) 
 REPRESENTATION_ITEM ( '' )  );
#3280 = CARTESIAN_POINT ( 'NONE',  ( -12.37436867076458036, -12.37436867076458036, 44.37436867076458213 ) ) ;
#3281 = EDGE_CURVE ( 'NONE', #5764, #1835, #5947, .T. ) ;
#3282 = ORIENTED_EDGE ( 'NONE', *, *, #3051, .T. ) ;
#3283 = VERTEX_POINT ( 'NONE', #4234 ) ;
#3284 = ORIENTED_EDGE ( 'NONE', *, *, #2475, .F. ) ;
#3285 = CARTESIAN_POINT ( 'NONE',  ( -5.000000000000000888, 6.123233995736767268E-16, 1.000000000000000000 ) ) ;
#3286 = DIRECTION ( 'NONE',  ( 1.000000000000000000, 0.000000000000000000, 0.000000000000000000 ) ) ;
#3287 = AXIS2_PLACEMENT_3D ( 'NONE', #560, #7139, #4125 ) ;
#3288 = CARTESIAN_POINT ( 'NONE',  ( -26.99999999999998934, 35.00000000000000000, 64.00000000000000000 ) ) ;
#3289 = DIRECTION ( 'NONE',  ( 0.5773502691896290617, -0.5773502691896225114, -0.5773502691896258421 ) ) ;
#3290 = LINE ( 'NONE', #8577, #4042 ) ;
#3291 = ORIENTED_EDGE ( 'NONE', *, *, #3410, .F. ) ;
#3292 = EDGE_CURVE ( 'NONE', #8189, #7366, #4289, .T. ) ;
#3293 = ORIENTED_EDGE ( 'NONE', *, *, #5348, .F. ) ;
#3294 = CARTESIAN_POINT ( 'NONE',  ( -30.99999999999996803, 0.000000000000000000, 32.00000000000000000 ) ) ;
#3295 = ORIENTED_EDGE ( 'NONE', *, *, #4417, .F. ) ;
#3296 = EDGE_CURVE ( 'NONE', #2294, #4010, #9471, .T. ) ;
#3297 = PLANE ( 'NONE',  #6244 ) ;
#3298 = CIRCLE ( 'NONE', #4213, 2.999999999999999112 ) ;
#3299 = ADVANCED_FACE ( 'NONE', ( #7984 ), #1396, .F. ) ;
#3300 = ADVANCED_FACE ( 'NONE', ( #2893 ), #8750, .T. ) ;
#3301 = EDGE_LOOP ( 'NONE', ( #5702, #5339, #4736, #8337 ) ) ;
#3302 = DIRECTION ( 'NONE',  ( 0.000000000000000000, 0.000000000000000000, 1.000000000000000000 ) ) ;
#3303 = DIRECTION ( 'NONE',  ( 0.000000000000000000, 0.000000000000000000, 1.000000000000000000 ) ) ;
#3304 = CARTESIAN_POINT ( 'NONE',  ( -38.00000000000000000, 44.39318849903271769, -6.762951650419153360 ) ) ;
#3305 = ORIENTED_EDGE ( 'NONE', *, *, #2259, .F. ) ;
#3306 = ORIENTED_EDGE ( 'NONE', *, *, #7386, .F. ) ;
#3307 = EDGE_CURVE ( 'NONE', #8690, #55, #8794, .T. ) ;
#3308 = AXIS2_PLACEMENT_3D ( 'NONE', #2973, #8929, #2408 ) ;
#3309 = EDGE_CURVE ( 'NONE', #31, #233, #8700, .T. ) ;
#3310 = DIRECTION ( 'NONE',  ( -1.000000000000000000, 0.000000000000000000, 0.000000000000000000 ) ) ;
#3311 = CARTESIAN_POINT ( 'NONE',  ( 5.000000000000000000, -9.628187502531647418E-13, -19.99999999999950262 ) ) ;
#3312 = AXIS2_PLACEMENT_3D ( 'NONE', #629, #3658, #4426 ) ;
#3313 = DIRECTION ( 'NONE',  ( 0.000000000000000000, 0.000000000000000000, 1.000000000000000000 ) ) ;
#3314 = ADVANCED_FACE ( 'NONE', ( #2934 ), #5917, .F. ) ;
#3315 = CARTESIAN_POINT ( 'NONE',  ( 32.00000000000000711, -29.99999999999996447, 64.00000000000000000 ) ) ;
#3316 = ORIENTED_EDGE ( 'NONE', *, *, #3994, .T. ) ;
#3317 = CARTESIAN_POINT ( 'NONE',  ( 28.50000000000000355, 7.347880794884123680E-16, 5.000000000000000000 ) ) ;
#3318 = ORIENTED_EDGE ( 'NONE', *, *, #6259, .F. ) ;
#3319 = VECTOR ( 'NONE', #79, 1000.000000000000000 ) ;
#3320 = LINE ( 'NONE', #4858, #8013 ) ;
#3321 = VECTOR ( 'NONE', #9388, 1000.000000000000000 ) ;
#3322 = CYLINDRICAL_SURFACE ( 'NONE', #6258, 15.00000000000000000 ) ;
#3323 = CARTESIAN_POINT ( 'NONE',  ( 60.00000000000000000, -15.90990257669733943, -57.09009742330271564 ) ) ;
#3324 = DIRECTION ( 'NONE',  ( -1.000000000000000000, -0.000000000000000000, -0.000000000000000000 ) ) ;
#3325 = CIRCLE ( 'NONE', #3939, 3.000000000000002665 ) ;
#3326 = VECTOR ( 'NONE', #8706, 1000.000000000000000 ) ;
#3327 = VERTEX_POINT ( 'NONE', #4432 ) ;
#3328 = EDGE_LOOP ( 'NONE', ( #3720, #2491, #6748, #683 ) ) ;
#3329 = DIRECTION ( 'NONE',  ( 1.000000000000000000, 0.000000000000000000, 0.000000000000000000 ) ) ;
#3330 = ORIENTED_EDGE ( 'NONE', *, *, #932, .T. ) ;
#3331 = AXIS2_PLACEMENT_3D ( 'NONE', #7876, #4221, #8551 ) ;
#3332 = CARTESIAN_POINT ( 'NONE',  ( 0.000000000000000000, 0.000000000000000000, 28.50000000000000355 ) ) ;
#3333 = VECTOR ( 'NONE', #7649, 1000.000000000000000 ) ;
#3334 = CARTESIAN_POINT ( 'NONE',  ( 4.000000000000000000, 14.14213562373112154, -14.14213562373077870 ) ) ;
#3335 = EDGE_CURVE ( 'NONE', #1694, #3651, #6643, .T. ) ;
#3336 = AXIS2_PLACEMENT_3D ( 'NONE', #723, #8699, #1392 ) ;
#3337 =( BOUNDED_CURVE ( )  B_SPLINE_CURVE ( 3, ( #9225, #1021, #974, #446 ),
 .UNSPECIFIED., .F., .F. ) 
 B_SPLINE_CURVE_WITH_KNOTS ( ( 4, 4 ),
 ( 4.334691002005220284, 4.712388980384689674 ),
 .UNSPECIFIED. ) 
 CURVE ( )  GEOMETRIC_REPRESENTATION_ITEM ( )  RATIONAL_B_SPLINE_CURVE ( ( 1.000000000000000000, 0.9881473088045076292, 0.9881473088045076292, 1.000000000000000000 ) ) 
 REPRESENTATION_ITEM ( '' )  );
#3338 = CARTESIAN_POINT ( 'NONE',  ( 4.000000000000000000, 7.653668647300657213, -17.72759065022447089 ) ) ;
#3339 = AXIS2_PLACEMENT_3D ( 'NONE', #7681, #7728, #4031 ) ;
#3340 = CARTESIAN_POINT ( 'NONE',  ( -12.37436867076458036, -12.37436867076458036, 44.37436867076458213 ) ) ;
#3341 = EDGE_CURVE ( 'NONE', #4201, #5210, #5643, .T. ) ;
#3342 = DIRECTION ( 'NONE',  ( 1.000000000000000000, 0.000000000000000000, 0.000000000000000000 ) ) ;
#3343 = ORIENTED_EDGE ( 'NONE', *, *, #4297, .T. ) ;
#3344 = ORIENTED_EDGE ( 'NONE', *, *, #1055, .T. ) ;
#3345 = CARTESIAN_POINT ( 'NONE',  ( 0.000000000000000000, 29.99999999999997158, 64.00000000000000000 ) ) ;
#3346 = ORIENTED_EDGE ( 'NONE', *, *, #3341, .F. ) ;
#3347 = CARTESIAN_POINT ( 'NONE',  ( 53.29490495164537833, -30.00000000000000000, -41.61356529332876875 ) ) ;
#3348 = LINE ( 'NONE', #3579, #4733 ) ;
#3349 = AXIS2_PLACEMENT_3D ( 'NONE', #7770, #7183, #1180 ) ;
#3350 = ORIENTED_EDGE ( 'NONE', *, *, #4314, .F. ) ;
#3351 = CARTESIAN_POINT ( 'NONE',  ( 16.50000000000000000, 2.356749903719115078E-13, 0.000000000000000000 ) ) ;
#3352 = LINE ( 'NONE', #9247, #2627 ) ;
#3353 = DIRECTION ( 'NONE',  ( -0.7071067811865487940, 0.000000000000000000, -0.7071067811865463515 ) ) ;
#3354 = CARTESIAN_POINT ( 'NONE',  ( -31.99999999999999289, 2.143131898507868643E-15, 49.50000000000000000 ) ) ;
#3355 = ORIENTED_EDGE ( 'NONE', *, *, #823, .F. ) ;
#3356 = AXIS2_PLACEMENT_3D ( 'NONE', #5143, #5969, #8130 ) ;
#3357 = EDGE_LOOP ( 'NONE', ( #2380, #7571 ) ) ;
#3358 = PRODUCT_DEFINITION ( 'UNKNOWN', '', #8980, #6056 ) ;
#3359 = EDGE_CURVE ( 'NONE', #152, #7481, #6108, .T. ) ;
#3360 = AXIS2_PLACEMENT_3D ( 'NONE', #1444, #6642, #5097 ) ;
#3361 = CARTESIAN_POINT ( 'NONE',  ( 0.000000000000000000, 9.603694566548697359E-13, 20.00000000000290612 ) ) ;
#3362 = ADVANCED_FACE ( 'NONE', ( #3754 ), #4248, .T. ) ;
#3363 = DIRECTION ( 'NONE',  ( -0.000000000000000000, -0.000000000000000000, -1.000000000000000000 ) ) ;
#3364 = PLANE ( 'NONE',  #7872 ) ;
#3365 = CARTESIAN_POINT ( 'NONE',  ( 34.25000000000000000, 43.00000000000000000, 25.00000000000000000 ) ) ;
#3366 = DIRECTION ( 'NONE',  ( 0.7071067811865454633, 0.5000000000000012212, 0.5000000000000016653 ) ) ;
#3367 = VERTEX_POINT ( 'NONE', #1496 ) ;
#3368 = ORIENTED_EDGE ( 'NONE', *, *, #2220, .F. ) ;
#3369 = CARTESIAN_POINT ( 'NONE',  ( 4.000000000000000000, -14.14213562373248401, -15.70213562373165850 ) ) ;
#3370 = EDGE_CURVE ( 'NONE', #2826, #8754, #8081, .T. ) ;
#3371 = CARTESIAN_POINT ( 'NONE',  ( 0.000000000000000000, 0.000000000000000000, 25.00000000000000000 ) ) ;
#3372 = CARTESIAN_POINT ( 'NONE',  ( 53.29490495164537833, -3.673940397442057600E-15, -70.00000000000000000 ) ) ;
#3373 = DIRECTION ( 'NONE',  ( 1.000000000000000000, 0.000000000000000000, 0.000000000000000000 ) ) ;
#3374 = DIRECTION ( 'NONE',  ( 0.000000000000000000, 0.9175556253099241832, 0.3976074376343005090 ) ) ;
#3375 = ORIENTED_EDGE ( 'NONE', *, *, #3751, .F. ) ;
#3376 = ORIENTED_EDGE ( 'NONE', *, *, #6480, .F. ) ;
#3377 = ORIENTED_EDGE ( 'NONE', *, *, #8257, .T. ) ;
#3378 = FACE_OUTER_BOUND ( 'NONE', #3181, .T. ) ;
#3379 = DIRECTION ( 'NONE',  ( 1.000000000000000000, 0.000000000000000000, 0.000000000000000000 ) ) ;
#3380 = AXIS2_PLACEMENT_3D ( 'NONE', #2342, #3102, #5168 ) ;
#3381 = LINE ( 'NONE', #6286, #9209 ) ;
#3382 = CARTESIAN_POINT ( 'NONE',  ( 1.571166602479410136E-13, -22.50000000000000355, 0.000000000000000000 ) ) ;
#3383 = DIRECTION ( 'NONE',  ( -0.000000000000000000, -0.000000000000000000, -1.000000000000000000 ) ) ;
#3384 = VERTEX_POINT ( 'NONE', #7447 ) ;
#3385 = VERTEX_POINT ( 'NONE', #105 ) ;
#3386 = CARTESIAN_POINT ( 'NONE',  ( 27.00000000000000000, 43.00000000000000000, 25.00000000000000000 ) ) ;
#3387 = VECTOR ( 'NONE', #1404, 999.9999999999998863 ) ;
#3388 = ORIENTED_EDGE ( 'NONE', *, *, #711, .T. ) ;
#3389 = DIRECTION ( 'NONE',  ( -0.000000000000000000, -0.000000000000000000, -1.000000000000000000 ) ) ;
#3390 = DIRECTION ( 'NONE',  ( 0.7071067811865481278, 0.000000000000000000, -0.7071067811865470176 ) ) ;
#3391 = ORIENTED_EDGE ( 'NONE', *, *, #2004, .T. ) ;
#3392 = DIRECTION ( 'NONE',  ( 0.7071067811865460184, 0.000000000000000000, 0.7071067811865489050 ) ) ;
#3393 = DIRECTION ( 'NONE',  ( 0.000000000000000000, 0.000000000000000000, -1.000000000000000000 ) ) ;
#3394 = CARTESIAN_POINT ( 'NONE',  ( -28.50000000000000355, 0.000000000000000000, 2.000000000000039080 ) ) ;
#3395 = LINE ( 'NONE', #4932, #2109 ) ;
#3396 = ORIENTED_EDGE ( 'NONE', *, *, #5118, .F. ) ;
#3397 = VERTEX_POINT ( 'NONE', #8133 ) ;
#3398 = VECTOR ( 'NONE', #2617, 1000.000000000000000 ) ;
#3399 = CONTEXT_DEPENDENT_SHAPE_REPRESENTATION ( #1171, #3460 ) ;
#3400 = EDGE_CURVE ( 'NONE', #2461, #4035, #642, .T. ) ;
#3401 = CARTESIAN_POINT ( 'NONE',  ( 0.000000000000000000, 2.143131898507868248E-15, -17.50000000000000000 ) ) ;
#3402 = DIRECTION ( 'NONE',  ( -1.000000000000000000, -0.000000000000000000, -0.000000000000000000 ) ) ;
#3403 = DIRECTION ( 'NONE',  ( 0.000000000000000000, 0.000000000000000000, 1.000000000000000000 ) ) ;
#3404 = EDGE_LOOP ( 'NONE', ( #6341, #4047 ) ) ;
#3405 = ORIENTED_EDGE ( 'NONE', *, *, #2255, .F. ) ;
#3406 = AXIS2_PLACEMENT_3D ( 'NONE', #5495, #8425, #3808 ) ;
#3407 = VERTEX_POINT ( 'NONE', #63 ) ;
#3408 = EDGE_CURVE ( 'NONE', #313, #6124, #16, .T. ) ;
#3409 = ORIENTED_EDGE ( 'NONE', *, *, #6002, .T. ) ;
#3410 = EDGE_CURVE ( 'NONE', #5804, #5944, #8397, .T. ) ;
#3411 = CARTESIAN_POINT ( 'NONE',  ( 4.000000000000000000, -18.47759065022790637, -7.653668647299759265 ) ) ;
#3412 = EDGE_CURVE ( 'NONE', #7436, #694, #7632, .T. ) ;
#3413 = EDGE_CURVE ( 'NONE', #2399, #3876, #2368, .T. ) ;
#3414 = DIRECTION ( 'NONE',  ( 0.000000000000000000, 0.000000000000000000, -1.000000000000000000 ) ) ;
#3415 = AXIS2_PLACEMENT_3D ( 'NONE', #7893, #8663, #2765 ) ;
#3416 = CARTESIAN_POINT ( 'NONE',  ( 53.29490495164537833, 15.90990257669733943, -82.90990257669729147 ) ) ;
#3417 = CARTESIAN_POINT ( 'NONE',  ( 5.000000000000000000, -14.14213562373248401, -14.14213562372942157 ) ) ;
#3418 = FACE_BOUND ( 'NONE', #2711, .T. ) ;
#3419 = ORIENTED_EDGE ( 'NONE', *, *, #4534, .F. ) ;
#3420 = ORIENTED_EDGE ( 'NONE', *, *, #5342, .T. ) ;
#3421 = DIRECTION ( 'NONE',  ( -1.000000000000000000, 0.000000000000000000, 0.000000000000000000 ) ) ;
#3422 = EDGE_LOOP ( 'NONE', ( #1531, #6213, #3686, #671 ) ) ;
#3423 = LINE ( 'NONE', #8612, #964 ) ;
#3424 = CONICAL_SURFACE ( 'NONE', #5735, 6.000000000000000888, 0.7853981633974498333 ) ;
#3425 = CARTESIAN_POINT ( 'NONE',  ( -37.00000000000000000, 13.96446609406729067, -95.00000000000000000 ) ) ;
#3426 = EDGE_CURVE ( 'NONE', #7603, #5380, #4099, .T. ) ;
#3427 = CYLINDRICAL_SURFACE ( 'NONE', #7537, 1.560000000000134168 ) ;
#3428 = CARTESIAN_POINT ( 'NONE',  ( 37.00000000000000000, -3.673940397442057600E-15, -55.00000000000000711 ) ) ;
#3429 = DIRECTION ( 'NONE',  ( 0.000000000000000000, 0.000000000000000000, -1.000000000000000000 ) ) ;
#3430 = VERTEX_POINT ( 'NONE', #5766 ) ;
#3431 = ORIENTED_EDGE ( 'NONE', *, *, #892, .T. ) ;
#3432 = CARTESIAN_POINT ( 'NONE',  ( -38.00000000000000711, 20.99999999999999289, -16.89999999999999858 ) ) ;
#3433 = VERTEX_POINT ( 'NONE', #759 ) ;
#3434 = CARTESIAN_POINT ( 'NONE',  ( 20.14434505884618432, -53.53579249963522102, -2.801156583491408281 ) ) ;
#3435 = CYLINDRICAL_SURFACE ( 'NONE', #2117, 17.50000000000000355 ) ;
#3436 = CARTESIAN_POINT ( 'NONE',  ( 17.50000000000000355, 0.000000000000000000, 49.50000000000000000 ) ) ;
#3437 = AXIS2_PLACEMENT_3D ( 'NONE', #4453, #7375, #840 ) ;
#3438 = CARTESIAN_POINT ( 'NONE',  ( -53.29490495164537833, 15.90990257669733943, -88.90990257669730568 ) ) ;
#3439 = VECTOR ( 'NONE', #5035, 999.9999999999998863 ) ;
#3440 = DIRECTION ( 'NONE',  ( -1.000000000000000000, 0.000000000000000000, 0.000000000000000000 ) ) ;
#3441 = CARTESIAN_POINT ( 'NONE',  ( 28.73308667824889184, 0.6789743538665647948, 1.739127150302864244 ) ) ;
#3442 = EDGE_LOOP ( 'NONE', ( #6588, #6847 ) ) ;
#3443 = AXIS2_PLACEMENT_3D ( 'NONE', #7782, #1874, #1466 ) ;
#3444 = ORIENTED_EDGE ( 'NONE', *, *, #4829, .F. ) ;
#3445 =( REPRESENTATION_RELATIONSHIP ('NONE','NONE', #1933, #8501 ) REPRESENTATION_RELATIONSHIP_WITH_TRANSFORMATION ( #4984 )SHAPE_REPRESENTATION_RELATIONSHIP( ) );
#3446 = EDGE_CURVE ( 'NONE', #9313, #5080, #9464, .T. ) ;
#3447 = LINE ( 'NONE', #9304, #8814 ) ;
#3448 = DIRECTION ( 'NONE',  ( 0.000000000000000000, 0.000000000000000000, -1.000000000000000000 ) ) ;
#3449 = CYLINDRICAL_SURFACE ( 'NONE', #6877, 7.250000000000002665 ) ;
#3450 = PRODUCT_DEFINITION_FORMATION_WITH_SPECIFIED_SOURCE ( 'ANY', '', #5855, .NOT_KNOWN. ) ;
#3451 = VERTEX_POINT ( 'NONE', #665 ) ;
#3452 = ADVANCED_FACE ( 'NONE', ( #1474 ), #5722, .F. ) ;
#3453 = VERTEX_POINT ( 'NONE', #2787 ) ;
#3454 = ORIENTED_EDGE ( 'NONE', *, *, #6961, .T. ) ;
#3455 = VERTEX_POINT ( 'NONE', #7973 ) ;
#3456 = FACE_BOUND ( 'NONE', #7514, .T. ) ;
#3457 = CARTESIAN_POINT ( 'NONE',  ( -3.000000000000000000, 22.50000000000000355, 15.00000000000000000 ) ) ;
#3458 = VECTOR ( 'NONE', #7206, 1000.000000000000000 ) ;
#3459 = DIRECTION ( 'NONE',  ( 0.000000000000000000, 0.000000000000000000, 1.000000000000000000 ) ) ;
#3460 = PRODUCT_DEFINITION_SHAPE ( 'NONE', 'NONE',  #9498 ) ;
#3461 = DIRECTION ( 'NONE',  ( -1.000000000000000000, 0.000000000000000000, 0.000000000000000000 ) ) ;
#3462 = CARTESIAN_POINT ( 'NONE',  ( 4.000000000000000000, 18.47759065022580316, -7.653668647301631545 ) ) ;
#3463 = ORIENTED_EDGE ( 'NONE', *, *, #2475, .T. ) ;
#3464 = VECTOR ( 'NONE', #3823, 1000.000000000000000 ) ;
#3465 = ORIENTED_EDGE ( 'NONE', *, *, #1806, .T. ) ;
#3466 = CARTESIAN_POINT ( 'NONE',  ( -28.78095890121428013, 80.45324141007792207, 43.95616229837704481 ) ) ;
#3467 = ORIENTED_EDGE ( 'NONE', *, *, #1661, .T. ) ;
#3468 = FACE_BOUND ( 'NONE', #5407, .T. ) ;
#3469 = DIRECTION ( 'NONE',  ( 0.000000000000000000, 0.000000000000000000, 1.000000000000000000 ) ) ;
#3471 = EDGE_CURVE ( 'NONE', #8884, #6290, #572, .T. ) ;
#3470 = CARTESIAN_POINT ( 'NONE',  ( 27.00000000000000000, -43.00000000000000000, 11.99999999999999645 ) ) ;
#3472 = DIRECTION ( 'NONE',  ( 0.000000000000000000, 0.000000000000000000, 1.000000000000000000 ) ) ;
#3473 = DIRECTION ( 'NONE',  ( -0.000000000000000000, -0.000000000000000000, -1.000000000000000000 ) ) ;
#3474 = ORIENTED_EDGE ( 'NONE', *, *, #3103, .F. ) ;
#3475 = VECTOR ( 'NONE', #8739, 1000.000000000000000 ) ;
#3476 = ORIENTED_EDGE ( 'NONE', *, *, #892, .F. ) ;
#3477 = CARTESIAN_POINT ( 'NONE',  ( -3.000000000000000000, 22.50000000000000355, 10.00000000000000000 ) ) ;
#3478 = COLOUR_RGB ( '',0.7921568627450980005, 0.8196078431372548767, 0.9333333333333333481 ) ;
#3479 = EDGE_LOOP ( 'NONE', ( #2227, #2996, #8265, #5805, #775, #2136, #4292, #8253, #3615, #4612, #4371, #7877, #931, #8734, #1409, #1669 ) ) ;
#3480 = AXIS2_PLACEMENT_3D ( 'NONE', #5240, #9463, #5093 ) ;
#3481 = DIRECTION ( 'NONE',  ( 0.000000000000000000, 0.000000000000000000, -1.000000000000000000 ) ) ;
#3482 = CARTESIAN_POINT ( 'NONE',  ( 22.50000000000000355, 2.356749903719115078E-13, 5.000000000000000000 ) ) ;
#3483 = DIRECTION ( 'NONE',  ( -0.7071067811865469066, 0.000000000000000000, -0.7071067811865481278 ) ) ;
#3484 = AXIS2_PLACEMENT_3D ( 'NONE', #5677, #569, #1279 ) ;
#3485 = PLANE ( 'NONE',  #8453 ) ;
#3486 = VECTOR ( 'NONE', #2687, 1000.000000000000000 ) ;
#3487 = CIRCLE ( 'NONE', #1495, 6.000000000000000888 ) ;
#3488 = CARTESIAN_POINT ( 'NONE',  ( 0.000000000000000000, 0.000000000000000000, 2.999999999999999112 ) ) ;
#3489 = CARTESIAN_POINT ( 'NONE',  ( 9.048619709455117288, -15.70011763207404520, 47.70011763207404698 ) ) ;
#3490 = ORIENTED_EDGE ( 'NONE', *, *, #1752, .T. ) ;
#3491 = ORIENTED_EDGE ( 'NONE', *, *, #3024, .F. ) ;
#3492 = CIRCLE ( 'NONE', #8262, 6.000000000000001776 ) ;
#3493 = CARTESIAN_POINT ( 'NONE',  ( -26.21170834203224231, 53.97171801779369105, -2.612255525622730001 ) ) ;
#3494 = CARTESIAN_POINT ( 'NONE',  ( 3.000000000000156763, -22.50000000000000355, 15.00000000000000000 ) ) ;
#3495 = AXIS2_PLACEMENT_3D ( 'NONE', #4394, #745, #6615 ) ;
#3496 = CARTESIAN_POINT ( 'NONE',  ( 0.000000000000000000, 18.47759065022580316, -7.653668647301631545 ) ) ;
#3497 = CIRCLE ( 'NONE', #589, 6.000000000000001776 ) ;
#3498 = DIRECTION ( 'NONE',  ( 0.5773502691896283956, 0.5773502691896228445, 0.5773502691896260641 ) ) ;
#3499 = FACE_OUTER_BOUND ( 'NONE', #2750, .T. ) ;
#3500 = ORIENTED_EDGE ( 'NONE', *, *, #7864, .F. ) ;
#3501 = ORIENTED_EDGE ( 'NONE', *, *, #5261, .F. ) ;
#3502 = EDGE_CURVE ( 'NONE', #6148, #5058, #1382, .T. ) ;
#3503 = ORIENTED_EDGE ( 'NONE', *, *, #9396, .T. ) ;
#3504 = AXIS2_PLACEMENT_3D ( 'NONE', #2047, #4836, #5028 ) ;
#3505 = ORIENTED_EDGE ( 'NONE', *, *, #5830, .F. ) ;
#3506 = ADVANCED_FACE ( 'NONE', ( #2829 ), #3182, .T. ) ;
#3507 = AXIS2_PLACEMENT_3D ( 'NONE', #7556, #9132, #1112 ) ;
#3508 = DIRECTION ( 'NONE',  ( 0.000000000000000000, -0.000000000000000000, -1.000000000000000000 ) ) ;
#3509 = LINE ( 'NONE', #5733, #3793 ) ;
#3510 = ADVANCED_FACE ( 'NONE', ( #9302 ), #3689, .T. ) ;
#3511 = DIRECTION ( 'NONE',  ( -1.000000000000000000, 0.000000000000000000, 0.000000000000000000 ) ) ;
#3512 = DIRECTION ( 'NONE',  ( -1.000000000000000000, -0.000000000000000000, -0.000000000000000000 ) ) ;
#3513 = FACE_OUTER_BOUND ( 'NONE', #1456, .T. ) ;
#3514 = VERTEX_POINT ( 'NONE', #9359 ) ;
#3515 = LINE ( 'NONE', #7261, #5014 ) ;
#3516 = VERTEX_POINT ( 'NONE', #5856 ) ;
#3517 = CARTESIAN_POINT ( 'NONE',  ( 1.571166602479410136E-13, -22.50000000000000355, 5.000000000000000000 ) ) ;
#3518 = EDGE_CURVE ( 'NONE', #2523, #3864, #8685, .T. ) ;
#3519 = DIRECTION ( 'NONE',  ( 0.000000000000000000, 0.000000000000000000, 1.000000000000000000 ) ) ;
#3520 = AXIS2_PLACEMENT_3D ( 'NONE', #676, #7442, #12 ) ;
#3521 = CARTESIAN_POINT ( 'NONE',  ( -16.49999999999999645, -7.782354204448209592E-14, 5.000000000000000000 ) ) ;
#3522 = CARTESIAN_POINT ( 'NONE',  ( -59.00000000000000000, 0.000000000000000000, 25.00000000000000000 ) ) ;
#3523 = CARTESIAN_POINT ( 'NONE',  ( 4.333301281932962823, -26.64999999999994529, 0.000000000000000000 ) ) ;
#3524 = ORIENTED_EDGE ( 'NONE', *, *, #8426, .F. ) ;
#3525 = ORIENTED_EDGE ( 'NONE', *, *, #1216, .T. ) ;
#3526 = LINE ( 'NONE', #3345, #9451 ) ;
#3527 = ORIENTED_EDGE ( 'NONE', *, *, #4892, .T. ) ;
#3528 = EDGE_CURVE ( 'NONE', #8532, #3216, #8638, .T. ) ;
#3529 = DIRECTION ( 'NONE',  ( 0.000000000000000000, 0.000000000000000000, 1.000000000000000000 ) ) ;
#3530 = EDGE_CURVE ( 'NONE', #6191, #4100, #6874, .T. ) ;
#3531 = DIRECTION ( 'NONE',  ( 0.000000000000000000, 0.000000000000000000, 1.000000000000000000 ) ) ;
#3532 = VECTOR ( 'NONE', #3728, 1000.000000000000000 ) ;
#3533 = CARTESIAN_POINT ( 'NONE',  ( 53.29490495164537833, -15.90990257669733943, -88.90990257669730568 ) ) ;
#3534 = EDGE_CURVE ( 'NONE', #2599, #1163, #7197, .T. ) ;
#3535 = ADVANCED_FACE ( 'NONE', ( #4320 ), #3019, .F. ) ;
#3536 = EDGE_CURVE ( 'NONE', #9413, #1969, #6723, .T. ) ;
#3537 = DIRECTION ( 'NONE',  ( 0.000000000000000000, 0.000000000000000000, -1.000000000000000000 ) ) ;
#3538 = CARTESIAN_POINT ( 'NONE',  ( 0.000000000000000000, 22.50000000000000355, 5.000000000000000000 ) ) ;
#3539 = VECTOR ( 'NONE', #7265, 1000.000000000000000 ) ;
#3540 = CARTESIAN_POINT ( 'NONE',  ( 1.571166602479410136E-13, -22.50000000000000355, 5.000000000000000000 ) ) ;
#3541 = EDGE_LOOP ( 'NONE', ( #8919, #9014, #267, #8673 ) ) ;
#3542 = EDGE_LOOP ( 'NONE', ( #4856, #8578 ) ) ;
#3543 = CARTESIAN_POINT ( 'NONE',  ( 60.00000000000000000, 29.99999999999999645, -82.50000000000000000 ) ) ;
#3544 = ITEM_DEFINED_TRANSFORMATION ( 'NONE', 'NONE', #1623,  #1614 ) ;
#3545 = VERTEX_POINT ( 'NONE', #8736 ) ;
#3546 = PRODUCT_DEFINITION_SHAPE ( 'NONE', 'NONE',  #9500 ) ;
#3547 = EDGE_CURVE ( 'NONE', #7512, #4808, #9449, .T. ) ;
#3548 = EDGE_CURVE ( 'NONE', #1211, #8690, #5083, .T. ) ;
#3549 = CARTESIAN_POINT ( 'NONE',  ( 41.99999999999999289, -30.00000000000000000, -100.0000000000000000 ) ) ;
#3550 = EDGE_CURVE ( 'NONE', #2406, #5958, #9406, .T. ) ;
#3551 = DIRECTION ( 'NONE',  ( -0.000000000000000000, -0.000000000000000000, -1.000000000000000000 ) ) ;
#3552 = AXIS2_PLACEMENT_3D ( 'NONE', #8605, #4146, #1251 ) ;
#3553 = VERTEX_POINT ( 'NONE', #4365 ) ;
#3554 = VERTEX_POINT ( 'NONE', #708 ) ;
#3555 = EDGE_LOOP ( 'NONE', ( #6424, #762 ) ) ;
#3556 = EDGE_LOOP ( 'NONE', ( #7152, #5024 ) ) ;
#3557 = CARTESIAN_POINT ( 'NONE',  ( 28.06144414093874673, -2.260912237343545073, 1.151721138160509916 ) ) ;
#3558 = CIRCLE ( 'NONE', #1406, 1.560000000000134168 ) ;
#3559 = DIRECTION ( 'NONE',  ( 1.000000000000000000, 0.000000000000000000, 0.000000000000000000 ) ) ;
#3560 = DIRECTION ( 'NONE',  ( 0.000000000000000000, 0.000000000000000000, 1.000000000000000000 ) ) ;
#3561 = FACE_OUTER_BOUND ( 'NONE', #2148, .T. ) ;
#3562 = AXIS2_PLACEMENT_3D ( 'NONE', #9277, #5648, #7989 ) ;
#3563 = CARTESIAN_POINT ( 'NONE',  ( 27.00000000000000355, 29.99999999999997158, 3.066586833366735950E-16 ) ) ;
#3564 = EDGE_LOOP ( 'NONE', ( #901, #7141 ) ) ;
#3565 = CYLINDRICAL_SURFACE ( 'NONE', #869, 0.7500000000000015543 ) ;
#3566 = EDGE_LOOP ( 'NONE', ( #2238, #1881, #7050, #850, #7106, #6058, #2076, #4992, #4253, #4056, #7097, #9243 ) ) ;
#3567 = CARTESIAN_POINT ( 'NONE',  ( 38.00000000000000000, 43.00000000000000000, -7.366666666666667140 ) ) ;
#3568 = AXIS2_PLACEMENT_3D ( 'NONE', #3332, #7215, #2712 ) ;
#3569 = CARTESIAN_POINT ( 'NONE',  ( 34.25000000000000000, -43.00000000000000000, 11.99999999999999645 ) ) ;
#3570 = CARTESIAN_POINT ( 'NONE',  ( 0.000000000000000000, 7.653668647302530381, 19.22759065022631830 ) ) ;
#3571 = LINE ( 'NONE', #3522, #5128 ) ;
#3572 = FACE_OUTER_BOUND ( 'NONE', #5101, .T. ) ;
#3573 = ORIENTED_EDGE ( 'NONE', *, *, #7351, .T. ) ;
#3574 = AXIS2_PLACEMENT_3D ( 'NONE', #6071, #2040, #7898 ) ;
#3575 = ORIENTED_EDGE ( 'NONE', *, *, #800, .T. ) ;
#3576 = CARTESIAN_POINT ( 'NONE',  ( -6.000000000000000888, 22.50000000000000355, 5.000000000000000000 ) ) ;
#3577 = ORIENTED_EDGE ( 'NONE', *, *, #6534, .T. ) ;
#3578 = CARTESIAN_POINT ( 'NONE',  ( -26.91700667250954027, -4.077589154199041666, 0.2225055604246516383 ) ) ;
#3579 = CARTESIAN_POINT ( 'NONE',  ( 5.000000000000000000, -18.47759065022712832, 8.403668647304948891 ) ) ;
#3580 = DIRECTION ( 'NONE',  ( -0.5773502691896283956, -0.000000000000000000, 0.8164965809277242581 ) ) ;
#3581 = LINE ( 'NONE', #609, #7835 ) ;
#3582 = VECTOR ( 'NONE', #3248, 1000.000000000000000 ) ;
#3583 =( BOUNDED_CURVE ( )  B_SPLINE_CURVE ( 3, ( #9417, #8075, #5967, #3604 ),
 .UNSPECIFIED., .F., .F. ) 
 B_SPLINE_CURVE_WITH_KNOTS ( ( 4, 4 ),
 ( 3.003391341741618259, 3.049711720517707114 ),
 .UNSPECIFIED. ) 
 CURVE ( )  GEOMETRIC_REPRESENTATION_ITEM ( )  RATIONAL_B_SPLINE_CURVE ( ( 1.000000000000000000, 0.9998212098678860293, 0.9998212098678860293, 1.000000000000000000 ) ) 
 REPRESENTATION_ITEM ( '' )  );
#3584 = DIRECTION ( 'NONE',  ( 0.000000000000000000, 0.000000000000000000, 1.000000000000000000 ) ) ;
#3585 = DIRECTION ( 'NONE',  ( -1.000000000000000000, -0.000000000000000000, -0.000000000000000000 ) ) ;
#3586 = EDGE_CURVE ( 'NONE', #6094, #3807, #1526, .T. ) ;
#3587 = ORIENTED_EDGE ( 'NONE', *, *, #4505, .F. ) ;
#3588 = EDGE_LOOP ( 'NONE', ( #5027, #8009, #4390, #2057, #2597, #7834 ) ) ;
#3589 = EDGE_CURVE ( 'NONE', #662, #1368, #5879, .T. ) ;
#3590 = CARTESIAN_POINT ( 'NONE',  ( 37.00000000000000000, -8.017766952966340455, -116.9822330470336453 ) ) ;
#3591 = ITEM_DEFINED_TRANSFORMATION ( 'NONE', 'NONE', #1157,  #1614 ) ;
#3592 = DIRECTION ( 'NONE',  ( 0.000000000000000000, 0.000000000000000000, 1.000000000000000000 ) ) ;
#3593 = AXIS2_PLACEMENT_3D ( 'NONE', #9226, #4098, #3374 ) ;
#3594 = VECTOR ( 'NONE', #6326, 1000.000000000000000 ) ;
#3595 = CARTESIAN_POINT ( 'NONE',  ( 53.29490495164537833, -30.00000000000000000, -100.0000000000000000 ) ) ;
#3596 = ORIENTED_EDGE ( 'NONE', *, *, #19, .F. ) ;
#3597 = ORIENTED_EDGE ( 'NONE', *, *, #6263, .F. ) ;
#3598 = ORIENTED_EDGE ( 'NONE', *, *, #5962, .T. ) ;
#3599 = EDGE_CURVE ( 'NONE', #5692, #4647, #905, .T. ) ;
#3600 = ORIENTED_EDGE ( 'NONE', *, *, #6843, .T. ) ;
#3601 = EDGE_CURVE ( 'NONE', #4792, #8301, #6272, .T. ) ;
#3602 = CARTESIAN_POINT ( 'NONE',  ( 22.50000000000000355, 0.000000000000000000, 5.000000000000000000 ) ) ;
#3603 = EDGE_CURVE ( 'NONE', #8277, #3283, #8923, .T. ) ;
#3604 = CARTESIAN_POINT ( 'NONE',  ( 51.96152422706632734, 30.00000000000000000, -80.85015119857381194 ) ) ;
#3605 = CARTESIAN_POINT ( 'NONE',  ( -28.48867854402453403, -0.4256064988643077363, 1.491066224433648557 ) ) ;
#3606 = CARTESIAN_POINT ( 'NONE',  ( -27.00000000000000000, -43.00000000000000000, 11.99999999999999645 ) ) ;
#3607 = AXIS2_PLACEMENT_3D ( 'NONE', #6238, #2449, #1671 ) ;
#3608 = EDGE_CURVE ( 'NONE', #8284, #8127, #5952, .T. ) ;
#3609 = CARTESIAN_POINT ( 'NONE',  ( -26.21170834203224231, 53.97171801779369105, -2.612255525622730001 ) ) ;
#3610 = CARTESIAN_POINT ( 'NONE',  ( -31.99999999999999289, 0.000000000000000000, 32.00000000000000000 ) ) ;
#3611 = DIRECTION ( 'NONE',  ( -1.000000000000000000, -0.000000000000000000, -0.000000000000000000 ) ) ;
#3612 = ORIENTED_EDGE ( 'NONE', *, *, #1418, .T. ) ;
#3613 = CARTESIAN_POINT ( 'NONE',  ( -17.49999999999999645, 4.703319286132086496, 14.49999999999999822 ) ) ;
#3614 = ORIENTED_EDGE ( 'NONE', *, *, #22, .F. ) ;
#3615 = ORIENTED_EDGE ( 'NONE', *, *, #7515, .T. ) ;
#3616 = FACE_OUTER_BOUND ( 'NONE', #578, .T. ) ;
#3617 = FACE_OUTER_BOUND ( 'NONE', #3723, .T. ) ;
#3618 = LINE ( 'NONE', #5064, #3539 ) ;
#3619 = CARTESIAN_POINT ( 'NONE',  ( 2.000000000000000000, 0.000000000000000000, 0.000000000000000000 ) ) ;
#3620 = AXIS2_PLACEMENT_3D ( 'NONE', #2144, #4262, #4929 ) ;
#3621 = CARTESIAN_POINT ( 'NONE',  ( 0.000000000000000000, 0.000000000000000000, 10.00000000000000000 ) ) ;
#3622 = VERTEX_POINT ( 'NONE', #4609 ) ;
#3623 = ORIENTED_EDGE ( 'NONE', *, *, #4754, .F. ) ;
#3624 = LINE ( 'NONE', #3767, #1169 ) ;
#3625 = ORIENTED_EDGE ( 'NONE', *, *, #8952, .F. ) ;
#3626 = EDGE_CURVE ( 'NONE', #5267, #6180, #2429, .T. ) ;
#3627 = CARTESIAN_POINT ( 'NONE',  ( -28.44339478698104884, -0.8493939025103932616, 1.455282208020838741 ) ) ;
#3628 = DIRECTION ( 'NONE',  ( -1.000000000000000000, 0.000000000000000000, 0.000000000000000000 ) ) ;
#3629 = DIRECTION ( 'NONE',  ( -0.000000000000000000, -0.000000000000000000, -1.000000000000000000 ) ) ;
#3630 = PRESENTATION_LAYER_ASSIGNMENT (  '', '', ( #6078 ) ) ;
#3631 =( REPRESENTATION_RELATIONSHIP ('NONE','NONE', #1933, #1625 ) REPRESENTATION_RELATIONSHIP_WITH_TRANSFORMATION ( #4760 )SHAPE_REPRESENTATION_RELATIONSHIP( ) );
#3632 = CYLINDRICAL_SURFACE ( 'NONE', #1079, 1.560000000002327303 ) ;
#3633 = EDGE_CURVE ( 'NONE', #2195, #4271, #2299, .T. ) ;
#3634 = DIRECTION ( 'NONE',  ( 0.7071067811865510144, 0.7071067811865441310, -0.000000000000000000 ) ) ;
#3635 = CLOSED_SHELL ( 'NONE', ( #5435, #3535, #3819, #2835, #4996, #8218, #2559, #1596, #9222, #5256, #8451, #2237, #5258, #9050, #1815, #4920, #141, #4341, #1633, #2832, #556, #8289, #7130, #9414, #6021, #7464, #7648, #8697, #2012, #5042, #4657, #7124, #7748, #1097, #2305, #8057, #5241, #2112, #1595, #3893, #6359, #8879, #8235, #1550, #7105, #3362 ) ) ;
#3636 = DIRECTION ( 'NONE',  ( 1.000000000000000000, -0.000000000000000000, -0.000000000000000000 ) ) ;
#3637 = CIRCLE ( 'NONE', #107, 15.66147716702868209 ) ;
#3638 = EDGE_LOOP ( 'NONE', ( #1365, #5442, #5398, #1254 ) ) ;
#3639 = ORIENTED_EDGE ( 'NONE', *, *, #8909, .F. ) ;
#3640 = CARTESIAN_POINT ( 'NONE',  ( -26.21170834203230982, -53.97171801779368394, -2.612255525622733554 ) ) ;
#3641 = FACE_OUTER_BOUND ( 'NONE', #1781, .T. ) ;
#3642 = CIRCLE ( 'NONE', #9156, 1.560000000002327303 ) ;
#3643 = AXIS2_PLACEMENT_3D ( 'NONE', #2828, #9355, #5040 ) ;
#3644 = CARTESIAN_POINT ( 'NONE',  ( -31.99999999999999289, 29.99999999999997868, 58.99999999999997158 ) ) ;
#3645 = VECTOR ( 'NONE', #157, 1000.000000000000114 ) ;
#3646 =( BOUNDED_CURVE ( )  B_SPLINE_CURVE ( 3, ( #314, #2525, #8286, #6762 ),
 .UNSPECIFIED., .F., .T. ) 
 B_SPLINE_CURVE_WITH_KNOTS ( ( 4, 4 ),
 ( 3.003391341741614262, 3.049711720517703117 ),
 .UNSPECIFIED. ) 
 CURVE ( )  GEOMETRIC_REPRESENTATION_ITEM ( )  RATIONAL_B_SPLINE_CURVE ( ( 1.000000000000000000, 0.9998212098678860293, 0.9998212098678860293, 1.000000000000000000 ) ) 
 REPRESENTATION_ITEM ( '' )  );
#3647 = AXIS2_PLACEMENT_3D ( 'NONE', #8344, #1767, #7006 ) ;
#3648 = CARTESIAN_POINT ( 'NONE',  ( 0.000000000000000000, 0.000000000000000000, 0.000000000000000000 ) ) ;
#3649 = DIRECTION ( 'NONE',  ( 0.000000000000000000, 0.000000000000000000, -1.000000000000000000 ) ) ;
#3650 = ORIENTED_EDGE ( 'NONE', *, *, #4300, .T. ) ;
#3651 = VERTEX_POINT ( 'NONE', #3116 ) ;
#3652 = ORIENTED_EDGE ( 'NONE', *, *, #8414, .T. ) ;
#3653 = EDGE_CURVE ( 'NONE', #8127, #5995, #147, .T. ) ;
#3654 = DIRECTION ( 'NONE',  ( -3.248947335124373738E-16, 0.9997175446104180629, -0.02376617340079580781 ) ) ;
#3655 = ORIENTED_EDGE ( 'NONE', *, *, #8431, .F. ) ;
#3656 = EDGE_CURVE ( 'NONE', #4735, #5058, #4263, .T. ) ;
#3657 = EDGE_CURVE ( 'NONE', #1974, #458, #9017, .T. ) ;
#3658 = DIRECTION ( 'NONE',  ( -1.000000000000000000, 0.000000000000000000, 0.000000000000000000 ) ) ;
#3659 = CARTESIAN_POINT ( 'NONE',  ( 4.000000000000000000, -9.626277053524975217E-13, -21.56000000000076966 ) ) ;
#3660 = DIRECTION ( 'NONE',  ( 0.000000000000000000, 0.000000000000000000, -1.000000000000000000 ) ) ;
#3661 = DIRECTION ( 'NONE',  ( -0.000000000000000000, -0.000000000000000000, -1.000000000000000000 ) ) ;
#3662 = CARTESIAN_POINT ( 'NONE',  ( 5.000000000000000000, -20.00000000000120437, 1.560000000004989174 ) ) ;
#3663 = CARTESIAN_POINT ( 'NONE',  ( 53.29490495164537833, 15.90990257669733943, -54.09009742330271564 ) ) ;
#3664 = AXIS2_PLACEMENT_3D ( 'NONE', #506, #3481, #1318 ) ;
#3665 = ORIENTED_EDGE ( 'NONE', *, *, #516, .F. ) ;
#3666 = CIRCLE ( 'NONE', #3210, 1.559999999999098552 ) ;
#3667 = DIRECTION ( 'NONE',  ( -1.000000000000000000, 0.000000000000000000, 0.000000000000000000 ) ) ;
#3668 = ORIENTED_EDGE ( 'NONE', *, *, #5611, .T. ) ;
#3669 = FACE_OUTER_BOUND ( 'NONE', #5252, .T. ) ;
#3670 = DIRECTION ( 'NONE',  ( 0.000000000000000000, 0.000000000000000000, -1.000000000000000000 ) ) ;
#3671 = VECTOR ( 'NONE', #6166, 1000.000000000000000 ) ;
#3672 = DIRECTION ( 'NONE',  ( -0.000000000000000000, -0.000000000000000000, -1.000000000000000000 ) ) ;
#3673 = DIRECTION ( 'NONE',  ( 0.000000000000000000, 0.000000000000000000, 1.000000000000000000 ) ) ;
#3674 = ORIENTED_EDGE ( 'NONE', *, *, #7147, .F. ) ;
#3675 = EDGE_LOOP ( 'NONE', ( #2963, #6802 ) ) ;
#3676 = CARTESIAN_POINT ( 'NONE',  ( 32.00000000000000711, -29.99999999999996447, 5.000000000000031974 ) ) ;
#3677 = ORIENTED_EDGE ( 'NONE', *, *, #6373, .F. ) ;
#3678 = DIRECTION ( 'NONE',  ( -0.000000000000000000, -0.000000000000000000, 1.000000000000000000 ) ) ;
#3679 = CARTESIAN_POINT ( 'NONE',  ( -34.25000000000000000, -43.00000000000000000, 11.99999999999999645 ) ) ;
#3680 = CARTESIAN_POINT ( 'NONE',  ( 5.000000000000000000, -7.653668647301985040, 17.72759065022987812 ) ) ;
#3681 = CARTESIAN_POINT ( 'NONE',  ( 2.750000000000006661, 0.7500000000000000000, 1.500000000000000000 ) ) ;
#3682 = CYLINDRICAL_SURFACE ( 'NONE', #6520, 2.999999999999999112 ) ;
#3683 = CARTESIAN_POINT ( 'NONE',  ( 0.000000000000000000, 0.000000000000000000, 10.00000000000000000 ) ) ;
#3684 = DIRECTION ( 'NONE',  ( -1.000000000000000000, -0.000000000000000000, -0.000000000000000000 ) ) ;
#3685 = VERTEX_POINT ( 'NONE', #6104 ) ;
#3686 = ORIENTED_EDGE ( 'NONE', *, *, #2846, .T. ) ;
#3687 = CARTESIAN_POINT ( 'NONE',  ( 0.000000000000000000, 20.00000000000120437, 7.412591687719288072E-13 ) ) ;
#3688 = VERTEX_POINT ( 'NONE', #9020 ) ;
#3689 = PLANE ( 'NONE',  #7166 ) ;
#3690 = VECTOR ( 'NONE', #8910, 1000.000000000000000 ) ;
#3691 = FACE_OUTER_BOUND ( 'NONE', #4591, .T. ) ;
#3692 = CARTESIAN_POINT ( 'NONE',  ( 0.000000000000000000, 0.000000000000000000, 10.00000000000000000 ) ) ;
#3693 = ORIENTED_EDGE ( 'NONE', *, *, #3975, .F. ) ;
#3694 = ORIENTED_EDGE ( 'NONE', *, *, #5679, .F. ) ;
#3695 = ORIENTED_EDGE ( 'NONE', *, *, #6843, .F. ) ;
#3696 = DIRECTION ( 'NONE',  ( -1.291822329104377007E-16, -0.9911323735125173728, 0.1328782080532535381 ) ) ;
#3697 = VERTEX_POINT ( 'NONE', #2456 ) ;
#3698 = CARTESIAN_POINT ( 'NONE',  ( -26.02777777777775370, -7.180166011355047395, 0.000000000000000000 ) ) ;
#3699 =( BOUNDED_CURVE ( )  B_SPLINE_CURVE ( 3, ( #1425, #8874, #5998, #3640 ),
 .UNSPECIFIED., .F., .T. ) 
 B_SPLINE_CURVE_WITH_KNOTS ( ( 4, 4 ),
 ( 1.570796326794896558, 3.069868295139984049 ),
 .UNSPECIFIED. ) 
 CURVE ( )  GEOMETRIC_REPRESENTATION_ITEM ( )  RATIONAL_B_SPLINE_CURVE ( ( 1.000000000000000000, 0.8213367208436757050, 0.8213367208436757050, 1.000000000000000000 ) ) 
 REPRESENTATION_ITEM ( '' )  );
#3700 = DIRECTION ( 'NONE',  ( -0.000000000000000000, -0.000000000000000000, -1.000000000000000000 ) ) ;
#3701 = ADVANCED_BREP_SHAPE_REPRESENTATION ( '', ( #171, #1614 ), #6385 ) ;
#3702 = CARTESIAN_POINT ( 'NONE',  ( -3.000000000000000000, -22.50000000000000355, 10.00000000000000000 ) ) ;
#3703 = PRODUCT_DEFINITION_SHAPE ( 'NONE', 'NONE',  #9048 ) ;
#3704 = CARTESIAN_POINT ( 'NONE',  ( -40.00000000000000000, 0.000000000000000000, -13.00000000000000533 ) ) ;
#3705 = CARTESIAN_POINT ( 'NONE',  ( 6.000000000000000888, 22.50000000000000355, 5.000000000000000000 ) ) ;
#3706 = ADVANCED_FACE ( 'NONE', ( #7579 ), #997, .F. ) ;
#3707 = CARTESIAN_POINT ( 'NONE',  ( 60.00000000000000000, -30.00000000000000355, -82.50000000000001421 ) ) ;
#3708 = EDGE_LOOP ( 'NONE', ( #1901, #6311, #832, #3719 ) ) ;
#3709 = EDGE_CURVE ( 'NONE', #8944, #334, #3988, .T. ) ;
#3710 = CARTESIAN_POINT ( 'NONE',  ( 16.00000000000000000, 43.00000000000000000, -7.366666666666667140 ) ) ;
#3711 = EDGE_CURVE ( 'NONE', #4945, #7976, #2580, .T. ) ;
#3712 = EDGE_CURVE ( 'NONE', #6154, #4625, #7478, .T. ) ;
#3713 = ORIENTED_EDGE ( 'NONE', *, *, #8303, .F. ) ;
#3714 = CIRCLE ( 'NONE', #2796, 3.000000000000002665 ) ;
#3715 = DIRECTION ( 'NONE',  ( 0.000000000000000000, 0.000000000000000000, -1.000000000000000000 ) ) ;
#3716 = DIRECTION ( 'NONE',  ( 0.000000000000000000, -1.000000000000000000, 0.000000000000000000 ) ) ;
#3717 = FACE_OUTER_BOUND ( 'NONE', #3566, .T. ) ;
#3718 = CARTESIAN_POINT ( 'NONE',  ( -62.09859669818813899, -30.00000000000000000, -66.51416582715449977 ) ) ;
#3719 = ORIENTED_EDGE ( 'NONE', *, *, #2143, .F. ) ;
#3720 = ORIENTED_EDGE ( 'NONE', *, *, #1216, .F. ) ;
#3721 = CARTESIAN_POINT ( 'NONE',  ( 1.463718181065913226, 28.32253049495584918, 1.359567973934761698 ) ) ;
#3722 = CIRCLE ( 'NONE', #1729, 1.560000000001466436 ) ;
#3723 = EDGE_LOOP ( 'NONE', ( #4121, #6996, #3954, #2396 ) ) ;
#3724 = DIRECTION ( 'NONE',  ( 0.000000000000000000, 0.000000000000000000, -1.000000000000000000 ) ) ;
#3725 = LINE ( 'NONE', #8046, #587 ) ;
#3726 = EDGE_CURVE ( 'NONE', #7789, #8983, #5427, .T. ) ;
#3727 = CARTESIAN_POINT ( 'NONE',  ( -27.00000000000000000, 43.00000000000000000, 25.00000000000000000 ) ) ;
#3728 = DIRECTION ( 'NONE',  ( 0.000000000000000000, 0.000000000000000000, -1.000000000000000000 ) ) ;
#3729 = DIRECTION ( 'NONE',  ( 0.7071067811865510144, 0.7071067811865441310, -0.000000000000000000 ) ) ;
#3730 = AXIS2_PLACEMENT_3D ( 'NONE', #3315, #8463, #1877 ) ;
#3731 = EDGE_CURVE ( 'NONE', #763, #991, #330, .T. ) ;
#3732 = DIRECTION ( 'NONE',  ( 0.000000000000000000, 0.000000000000000000, 1.000000000000000000 ) ) ;
#3733 = DIRECTION ( 'NONE',  ( -1.000000000000000000, 0.000000000000000000, 0.000000000000000000 ) ) ;
#3734 = ORIENTED_EDGE ( 'NONE', *, *, #2823, .F. ) ;
#3735 = ORIENTED_EDGE ( 'NONE', *, *, #1838, .T. ) ;
#3736 = DIRECTION ( 'NONE',  ( 0.000000000000000000, 0.000000000000000000, -1.000000000000000000 ) ) ;
#3737 = ORIENTED_EDGE ( 'NONE', *, *, #9345, .T. ) ;
#3738 = CARTESIAN_POINT ( 'NONE',  ( -1.687492729851148177, 28.61614266785989358, 1.663948857909935075 ) ) ;
#3739 = DIRECTION ( 'NONE',  ( -1.000000000000000000, 0.000000000000000000, 0.000000000000000000 ) ) ;
#3740 = UNCERTAINTY_MEASURE_WITH_UNIT (LENGTH_MEASURE( 1.000000000000000082E-05 ), #8042, 'distance_accuracy_value', 'NONE');
#3741 = LINE ( 'NONE', #854, #3475 ) ;
#3742 = VERTEX_POINT ( 'NONE', #1911 ) ;
#3743 = ORIENTED_EDGE ( 'NONE', *, *, #6871, .T. ) ;
#3744 = DIRECTION ( 'NONE',  ( 4.748805515486509421E-17, 0.9997175446104179519, -0.02376617340079592577 ) ) ;
#3745 = ADVANCED_FACE ( 'NONE', ( #4888 ), #7792, .T. ) ;
#3746 = AXIS2_PLACEMENT_3D ( 'NONE', #7731, #2737, #5668 ) ;
#3747 = LINE ( 'NONE', #7349, #8683 ) ;
#3748 = CARTESIAN_POINT ( 'NONE',  ( -34.25000000000000000, 43.00000000000000000, 11.99999999999999645 ) ) ;
#3749 = AXIS2_PLACEMENT_3D ( 'NONE', #5653, #1261, #4966 ) ;
#3750 = DIRECTION ( 'NONE',  ( 0.000000000000000000, 0.000000000000000000, -1.000000000000000000 ) ) ;
#3751 = EDGE_CURVE ( 'NONE', #943, #4838, #4110, .T. ) ;
#3752 = DIRECTION ( 'NONE',  ( 0.000000000000000000, 0.000000000000000000, -1.000000000000000000 ) ) ;
#3753 = DIRECTION ( 'NONE',  ( -0.7071067811865441310, -0.5000000000000026645, 0.5000000000000023315 ) ) ;
#3754 = FACE_OUTER_BOUND ( 'NONE', #4787, .T. ) ;
#3755 = VERTEX_POINT ( 'NONE', #1048 ) ;
#3756 = CARTESIAN_POINT ( 'NONE',  ( 0.000000000000000000, -22.50000000000000355, 2.000000000000013767 ) ) ;
#3757 = VECTOR ( 'NONE', #6260, 1000.000000000000000 ) ;
#3758 = EDGE_LOOP ( 'NONE', ( #6968, #1482 ) ) ;
#3759 =( REPRESENTATION_RELATIONSHIP ('NONE','NONE', #1933, #3963 ) REPRESENTATION_RELATIONSHIP_WITH_TRANSFORMATION ( #3217 )SHAPE_REPRESENTATION_RELATIONSHIP( ) );
#3760 = CARTESIAN_POINT ( 'NONE',  ( -28.50000000000000000, -7.855833971761515132E-14, 1.500000000000037748 ) ) ;
#3761 = DIRECTION ( 'NONE',  ( 1.000000000000000000, 0.000000000000000000, 0.000000000000000000 ) ) ;
#3762 = CARTESIAN_POINT ( 'NONE',  ( -31.99999999999999289, -34.99999999999999289, 58.99999999999997158 ) ) ;
#3763 = CYLINDRICAL_SURFACE ( 'NONE', #2646, 3.000000000000002665 ) ;
#3764 = ORIENTED_EDGE ( 'NONE', *, *, #7665, .F. ) ;
#3765 = VERTEX_POINT ( 'NONE', #3256 ) ;
#3766 = ORIENTED_EDGE ( 'NONE', *, *, #2306, .T. ) ;
#3767 = CARTESIAN_POINT ( 'NONE',  ( 6.000000000000157208, -22.50000000000000355, 5.000000000000000000 ) ) ;
#3768 = EDGE_LOOP ( 'NONE', ( #1025, #96, #9087, #3596 ) ) ;
#3769 = CARTESIAN_POINT ( 'NONE',  ( -28.61406079152386894, 10.49089634068029575, -86.61406079152385473 ) ) ;
#3770 = DIRECTION ( 'NONE',  ( 0.000000000000000000, 0.000000000000000000, -1.000000000000000000 ) ) ;
#3771 = ADVANCED_FACE ( 'NONE', ( #6916 ), #4703, .F. ) ;
#3772 = CARTESIAN_POINT ( 'NONE',  ( 57.72192878071319910, 19.00148731544556568, -33.94573509506513176 ) ) ;
#3773 = CYLINDRICAL_SURFACE ( 'NONE', #929, 13.66147716702868031 ) ;
#3774 = CIRCLE ( 'NONE', #395, 11.00000000000000711 ) ;
#3775 = CARTESIAN_POINT ( 'NONE',  ( 0.000000000000000000, 0.000000000000000000, 1.000000000000000000 ) ) ;
#3776 = CARTESIAN_POINT ( 'NONE',  ( 15.00000000000000000, 1.836970198721029589E-15, 26.99999999999999289 ) ) ;
#3777 = CARTESIAN_POINT ( 'NONE',  ( 28.75000000000001776, 7.654042494438380704E-16, 1.750000000000019762 ) ) ;
#3778 = EDGE_LOOP ( 'NONE', ( #7425, #7340, #2935, #3346 ) ) ;
#3779 = VERTEX_POINT ( 'NONE', #6198 ) ;
#3780 = CIRCLE ( 'NONE', #2564, 1.560000000001466436 ) ;
#3781 = CARTESIAN_POINT ( 'NONE',  ( 5.000000000000000000, 18.47759065022658120, 6.903668647304224137 ) ) ;
#3782 =( GEOMETRIC_REPRESENTATION_CONTEXT ( 3 ) GLOBAL_UNCERTAINTY_ASSIGNED_CONTEXT ( ( #5956 ) ) GLOBAL_UNIT_ASSIGNED_CONTEXT ( ( #1747, #1606, #4015 ) ) REPRESENTATION_CONTEXT ( 'NONE', 'WORKASPACE' ) );
#3783 = ORIENTED_EDGE ( 'NONE', *, *, #6373, .T. ) ;
#3784 = PRODUCT_DEFINITION_SHAPE ( 'NONE', 'NONE',  #9478 ) ;
#3785 = CARTESIAN_POINT ( 'NONE',  ( -41.99999999999999289, -30.00000000000000000, -100.0000000000000000 ) ) ;
#3786 = CARTESIAN_POINT ( 'NONE',  ( 5.000000000000000000, -20.00000000000120437, 2.661998082081668380E-12 ) ) ;
#3787 = LINE ( 'NONE', #6677, #567 ) ;
#3788 = CIRCLE ( 'NONE', #6561, 0.7500000000000006661 ) ;
#3789 = ORIENTED_EDGE ( 'NONE', *, *, #9316, .F. ) ;
#3790 = ORIENTED_EDGE ( 'NONE', *, *, #9361, .F. ) ;
#3791 = DIRECTION ( 'NONE',  ( 1.000000000000000000, 0.000000000000000000, 0.000000000000000000 ) ) ;
#3792 = AXIS2_PLACEMENT_3D ( 'NONE', #3687, #2917, #4556 ) ;
#3793 = VECTOR ( 'NONE', #2756, 1000.000000000000000 ) ;
#3794 = CARTESIAN_POINT ( 'NONE',  ( 26.65000000000001634, -4.333301281932499194, 0.000000000000000000 ) ) ;
#3795 = CARTESIAN_POINT ( 'NONE',  ( 12.37436867076458036, -12.37436867076458036, 44.37436867076458213 ) ) ;
#3796 = AXIS2_PLACEMENT_3D ( 'NONE', #7819, #5473, #8398 ) ;
#3797 = DIRECTION ( 'NONE',  ( 0.000000000000000000, 0.000000000000000000, -1.000000000000000000 ) ) ;
#3798 = CIRCLE ( 'NONE', #2266, 12.50000000000000000 ) ;
#3799 = CARTESIAN_POINT ( 'NONE',  ( 31.00000000000002132, 0.000000000000000000, 14.49999999999999467 ) ) ;
#3800 = DIRECTION ( 'NONE',  ( -1.000000000000000000, -0.000000000000000000, -0.000000000000000000 ) ) ;
#3801 = AXIS2_PLACEMENT_3D ( 'NONE', #4697, #990, #3110 ) ;
#3802 = DIRECTION ( 'NONE',  ( 1.000000000000000000, 0.000000000000000000, 0.000000000000000000 ) ) ;
#3803 = LINE ( 'NONE', #5441, #3890 ) ;
#3804 = ORIENTED_EDGE ( 'NONE', *, *, #2919, .T. ) ;
#3805 = CARTESIAN_POINT ( 'NONE',  ( 0.000000000000000000, 0.000000000000000000, 27.50000000000000355 ) ) ;
#3806 = CIRCLE ( 'NONE', #7032, 3.000000000000002665 ) ;
#3807 = VERTEX_POINT ( 'NONE', #9067 ) ;
#3808 = DIRECTION ( 'NONE',  ( -1.000000000000000000, 0.000000000000000000, 0.000000000000000000 ) ) ;
#3809 = EDGE_CURVE ( 'NONE', #4380, #1809, #8193, .T. ) ;
#3810 = DIRECTION ( 'NONE',  ( -1.000000000000000000, -0.000000000000000000, -0.000000000000000000 ) ) ;
#3811 = DIRECTION ( 'NONE',  ( 1.000000000000000000, 0.000000000000000000, 0.000000000000000000 ) ) ;
#3812 = CARTESIAN_POINT ( 'NONE',  ( -31.99999999999999289, 0.000000000000000000, 32.00000000000000000 ) ) ;
#3813 = CIRCLE ( 'NONE', #5973, 3.000000000000000000 ) ;
#3814 = CIRCLE ( 'NONE', #1053, 12.50000000000000000 ) ;
#3815 = ORIENTED_EDGE ( 'NONE', *, *, #3180, .T. ) ;
#3816 = ORIENTED_EDGE ( 'NONE', *, *, #8322, .F. ) ;
#3817 = ORIENTED_EDGE ( 'NONE', *, *, #8614, .T. ) ;
#3818 = EDGE_LOOP ( 'NONE', ( #8375, #7416, #5415, #8477, #3694 ) ) ;
#3819 = ADVANCED_FACE ( 'NONE', ( #415 ), #6312, .T. ) ;
#3820 = CARTESIAN_POINT ( 'NONE',  ( 60.00000000000000000, -15.90990257669733943, -51.09009742330271564 ) ) ;
#3821 = FACE_BOUND ( 'NONE', #3442, .T. ) ;
#3822 = VECTOR ( 'NONE', #6836, 1000.000000000000000 ) ;
#3823 = DIRECTION ( 'NONE',  ( -1.000000000000000000, -0.000000000000000000, -0.000000000000000000 ) ) ;
#3824 = CARTESIAN_POINT ( 'NONE',  ( 51.96152422706632734, -30.00000000000000000, -134.0000000000000284 ) ) ;
#3825 = PLANE ( 'NONE',  #3593 ) ;
#3826 = FACE_OUTER_BOUND ( 'NONE', #6497, .T. ) ;
#3827 = ORIENTED_EDGE ( 'NONE', *, *, #633, .F. ) ;
#3828 = EDGE_CURVE ( 'NONE', #2159, #3262, #6155, .T. ) ;
#3829 = ORIENTED_EDGE ( 'NONE', *, *, #6438, .T. ) ;
#3830 = EDGE_CURVE ( 'NONE', #2599, #7510, #3352, .T. ) ;
#3831 = DIRECTION ( 'NONE',  ( 0.000000000000000000, -1.000000000000000000, 0.000000000000000000 ) ) ;
#3832 = LINE ( 'NONE', #4502, #1665 ) ;
#3833 = EDGE_CURVE ( 'NONE', #8566, #8795, #6297, .T. ) ;
#3834 = EDGE_CURVE ( 'NONE', #6367, #1132, #8450, .T. ) ;
#3835 = ORIENTED_EDGE ( 'NONE', *, *, #5611, .F. ) ;
#3836 = CARTESIAN_POINT ( 'NONE',  ( 5.000000000000000000, 7.653668647302530381, 17.72759065022973246 ) ) ;
#3837 = VECTOR ( 'NONE', #9383, 999.9999999999998863 ) ;
#3838 = CARTESIAN_POINT ( 'NONE',  ( 15.00000000000000000, 1.836970198721029589E-15, 20.00000000000000000 ) ) ;
#3839 = UNCERTAINTY_MEASURE_WITH_UNIT (LENGTH_MEASURE( 1.000000000000000082E-05 ), #5393, 'distance_accuracy_value', 'NONE');
#3840 = CARTESIAN_POINT ( 'NONE',  ( 6.697288230627575167, -26.42764960499151528, 0.2570604603516986608 ) ) ;
#3841 = ORIENTED_EDGE ( 'NONE', *, *, #5540, .T. ) ;
#3842 = ORIENTED_EDGE ( 'NONE', *, *, #2964, .F. ) ;
#3843 = EDGE_CURVE ( 'NONE', #5058, #4735, #621, .T. ) ;
#3844 = PRODUCT_CONTEXT ( 'NONE', #2480, 'mechanical' ) ;
#3845 = ADVANCED_FACE ( 'NONE', ( #1184 ), #469, .F. ) ;
#3846 = CARTESIAN_POINT ( 'NONE',  ( -31.99999999999999289, -29.99999999999996447, 58.99999999999997158 ) ) ;
#3847 = ADVANCED_FACE ( 'NONE', ( #5617, #8540 ), #2003, .T. ) ;
#3848 = CARTESIAN_POINT ( 'NONE',  ( -53.29490495164537833, 18.67545040036925386, -90.28901569369799063 ) ) ;
#3849 = DIRECTION ( 'NONE',  ( 0.000000000000000000, 0.000000000000000000, -1.000000000000000000 ) ) ;
#3850 = CARTESIAN_POINT ( 'NONE',  ( -14.49999999999998401, 0.000000000000000000, 27.50000000000000355 ) ) ;
#3851 = CARTESIAN_POINT ( 'NONE',  ( -31.99999999999999289, 0.000000000000000000, 32.00000000000000000 ) ) ;
#3852 = CARTESIAN_POINT ( 'NONE',  ( -1.665361372754348812, -28.26799472218765175, 1.316292147329112483 ) ) ;
#3853 = AXIS2_PLACEMENT_3D ( 'NONE', #7851, #7895, #8716 ) ;
#3854 = VERTEX_POINT ( 'NONE', #7906 ) ;
#3855 = SURFACE_STYLE_FILL_AREA ( #6170 ) ;
#3856 = ORIENTED_EDGE ( 'NONE', *, *, #8353, .F. ) ;
#3857 = PLANE ( 'NONE',  #4037 ) ;
#3858 = DIRECTION ( 'NONE',  ( -0.7071067811865486830, 0.000000000000000000, -0.7071067811865464625 ) ) ;
#3859 = DIRECTION ( 'NONE',  ( 0.000000000000000000, -0.3976074376343005090, -0.9175556253099241832 ) ) ;
#3860 = CARTESIAN_POINT ( 'NONE',  ( -12.37436867076458036, 12.37436867076458036, 44.37436867076458213 ) ) ;
#3861 = VERTEX_POINT ( 'NONE', #7137 ) ;
#3862 = VECTOR ( 'NONE', #28, 1000.000000000000000 ) ;
#3863 = ORIENTED_EDGE ( 'NONE', *, *, #2717, .F. ) ;
#3864 = VERTEX_POINT ( 'NONE', #559 ) ;
#3865 = ORIENTED_EDGE ( 'NONE', *, *, #5990, .F. ) ;
#3866 = DIRECTION ( 'NONE',  ( -0.000000000000000000, -0.000000000000000000, -1.000000000000000000 ) ) ;
#3867 = DIRECTION ( 'NONE',  ( -0.7071067811865460184, 0.000000000000000000, -0.7071067811865489050 ) ) ;
#3868 = CARTESIAN_POINT ( 'NONE',  ( 22.50000000000000355, 2.356749903719115078E-13, 5.000000000000000000 ) ) ;
#3869 = EDGE_CURVE ( 'NONE', #2294, #9473, #4208, .T. ) ;
#3870 = MECHANICAL_DESIGN_GEOMETRIC_PRESENTATION_REPRESENTATION (  '', ( #2341 ), #1195 ) ;
#3871 = DIRECTION ( 'NONE',  ( -1.000000000000000000, 0.000000000000000000, 0.000000000000000000 ) ) ;
#3872 = LINE ( 'NONE', #8868, #2683 ) ;
#3873 = PRESENTATION_STYLE_ASSIGNMENT (( #181 ) ) ;
#3874 = CIRCLE ( 'NONE', #5096, 26.99999999999997868 ) ;
#3875 = DIRECTION ( 'NONE',  ( -0.000000000000000000, -0.000000000000000000, -1.000000000000000000 ) ) ;
#3876 = VERTEX_POINT ( 'NONE', #3438 ) ;
#3877 = EDGE_LOOP ( 'NONE', ( #4438, #1808 ) ) ;
#3878 = DIRECTION ( 'NONE',  ( -1.000000000000000000, 0.000000000000000000, 0.000000000000000000 ) ) ;
#3879 = ORIENTED_EDGE ( 'NONE', *, *, #4233, .T. ) ;
#3880 = FACE_BOUND ( 'NONE', #9365, .T. ) ;
#3881 = ORIENTED_EDGE ( 'NONE', *, *, #3502, .F. ) ;
#3882 = AXIS2_PLACEMENT_3D ( 'NONE', #4059, #1705, #7610 ) ;
#3883 = DIRECTION ( 'NONE',  ( 0.000000000000000000, 0.000000000000000000, -1.000000000000000000 ) ) ;
#3884 = ADVANCED_FACE ( 'NONE', ( #2778 ), #6460, .T. ) ;
#3885 = CARTESIAN_POINT ( 'NONE',  ( 0.000000000000000000, 0.000000000000000000, 0.000000000000000000 ) ) ;
#3886 = ADVANCED_FACE ( 'NONE', ( #1374 ), #3485, .F. ) ;
#3887 = CARTESIAN_POINT ( 'NONE',  ( -9.048619709455111959, -15.70011763207404876, 47.70011763207404698 ) ) ;
#3888 = VERTEX_POINT ( 'NONE', #1323 ) ;
#3889 = EDGE_LOOP ( 'NONE', ( #6930, #7191, #1329, #1317 ) ) ;
#3890 = VECTOR ( 'NONE', #4671, 1000.000000000000000 ) ;
#3891 = DIRECTION ( 'NONE',  ( 0.000000000000000000, 0.000000000000000000, 1.000000000000000000 ) ) ;
#3892 = DIRECTION ( 'NONE',  ( 0.000000000000000000, -0.000000000000000000, 1.000000000000000000 ) ) ;
#3893 = ADVANCED_FACE ( 'NONE', ( #7187 ), #6772, .F. ) ;
#3894 = DIRECTION ( 'NONE',  ( -0.7071067811865490160, -0.7071067811865461294, -0.000000000000000000 ) ) ;
#3895 = PRESENTATION_STYLE_ASSIGNMENT (( #6119 ) ) ;
#3896 = CARTESIAN_POINT ( 'NONE',  ( 0.000000000000000000, 0.000000000000000000, 10.00000000000000000 ) ) ;
#3897 = EDGE_CURVE ( 'NONE', #2826, #6270, #2145, .T. ) ;
#3898 = CARTESIAN_POINT ( 'NONE',  ( 51.96152422706632734, 30.00000000000000000, -80.85015119857381194 ) ) ;
#3899 = ORIENTED_EDGE ( 'NONE', *, *, #728, .T. ) ;
#3900 = CIRCLE ( 'NONE', #4061, 7.250000000000002665 ) ;
#3901 = DIRECTION ( 'NONE',  ( -1.000000000000000000, 0.000000000000000000, 0.000000000000000000 ) ) ;
#3902 = ORIENTED_EDGE ( 'NONE', *, *, #1535, .T. ) ;
#3903 = CARTESIAN_POINT ( 'NONE',  ( -3.000000000000000000, 22.50000000000000355, 5.000000000000000000 ) ) ;
#3904 = AXIS2_PLACEMENT_3D ( 'NONE', #3496, #5120, #7329 ) ;
#3905 = CARTESIAN_POINT ( 'NONE',  ( 19.74999999999999645, -43.00000000000000000, 25.00000000000000000 ) ) ;
#3906 = DIRECTION ( 'NONE',  ( 0.000000000000000000, 0.000000000000000000, 1.000000000000000000 ) ) ;
#3907 = CIRCLE ( 'NONE', #2982, 0.7500000000001906253 ) ;
#3908 = DIRECTION ( 'NONE',  ( 1.000000000000000000, 0.000000000000000000, 0.000000000000000000 ) ) ;
#3909 = ORIENTED_EDGE ( 'NONE', *, *, #4070, .T. ) ;
#3910 = CIRCLE ( 'NONE', #9266, 30.00000000000000000 ) ;
#3911 = ORIENTED_EDGE ( 'NONE', *, *, #8006, .F. ) ;
#3912 = ORIENTED_EDGE ( 'NONE', *, *, #594, .T. ) ;
#3913 = VERTEX_POINT ( 'NONE', #8772 ) ;
#3914 = CARTESIAN_POINT ( 'NONE',  ( 57.72192878071321331, -19.00148731544555147, -33.94573509506509623 ) ) ;
#3915 = LINE ( 'NONE', #1849, #6801 ) ;
#3916 = DIRECTION ( 'NONE',  ( -0.000000000000000000, -1.000000000000000000, -0.000000000000000000 ) ) ;
#3917 = CARTESIAN_POINT ( 'NONE',  ( 53.29490495164537833, -15.90990257669733943, -85.90990257669729147 ) ) ;
#3918 = DIRECTION ( 'NONE',  ( 0.000000000000000000, 0.000000000000000000, -1.000000000000000000 ) ) ;
#3919 = AXIS2_PLACEMENT_3D ( 'NONE', #1256, #539, #7754 ) ;
#3920 = CARTESIAN_POINT ( 'NONE',  ( 0.000000000000000000, 0.000000000000000000, 20.00000000000000000 ) ) ;
#3921 = CARTESIAN_POINT ( 'NONE',  ( -19.74999999999999645, -43.00000000000000000, 25.00000000000000000 ) ) ;
#3922 = ADVANCED_FACE ( 'NONE', ( #6433 ), #5667, .T. ) ;
#3923 = EDGE_LOOP ( 'NONE', ( #4172, #7155 ) ) ;
#3924 = ORIENTED_EDGE ( 'NONE', *, *, #7422, .F. ) ;
#3925 = DIRECTION ( 'NONE',  ( -1.000000000000000000, 0.000000000000000000, 0.000000000000000000 ) ) ;
#3926 = VERTEX_POINT ( 'NONE', #8005 ) ;
#3927 = DIRECTION ( 'NONE',  ( -0.000000000000000000, -0.000000000000000000, -1.000000000000000000 ) ) ;
#3928 = DIRECTION ( 'NONE',  ( -2.775557561562892584E-17, -0.7071067811865493491, 0.7071067811865456854 ) ) ;
#3929 = ORIENTED_EDGE ( 'NONE', *, *, #6259, .T. ) ;
#3930 = VECTOR ( 'NONE', #1959, 1000.000000000000000 ) ;
#3931 = EDGE_CURVE ( 'NONE', #9459, #3236, #2188, .T. ) ;
#3932 = CARTESIAN_POINT ( 'NONE',  ( -26.21170834203230982, -53.97171801779368394, -2.612255525622733554 ) ) ;
#3933 = CARTESIAN_POINT ( 'NONE',  ( 0.000000000000000000, 0.000000000000000000, 25.00000000000000000 ) ) ;
#3934 = DIRECTION ( 'NONE',  ( 0.7071067811865454633, 0.7071067811865494601, 0.000000000000000000 ) ) ;
#3935 = VECTOR ( 'NONE', #4665, 1000.000000000000000 ) ;
#3936 = VERTEX_POINT ( 'NONE', #9349 ) ;
#3937 = ORIENTED_EDGE ( 'NONE', *, *, #8431, .T. ) ;
#3938 = ITEM_DEFINED_TRANSFORMATION ( 'NONE', 'NONE', #1930,  #1614 ) ;
#3939 = AXIS2_PLACEMENT_3D ( 'NONE', #5100, #2985, #9424 ) ;
#3940 = CARTESIAN_POINT ( 'NONE',  ( 2.143131898507868248E-15, -34.00000000000001421, 14.49999999999999822 ) ) ;
#3941 = CIRCLE ( 'NONE', #5157, 0.7500000000012114754 ) ;
#3942 =( REPRESENTATION_RELATIONSHIP ('NONE','NONE', #1933, #6298 ) REPRESENTATION_RELATIONSHIP_WITH_TRANSFORMATION ( #7687 )SHAPE_REPRESENTATION_RELATIONSHIP( ) );
#3943 = CARTESIAN_POINT ( 'NONE',  ( 0.000000000000000000, 17.50000000000000000, 49.50000000000000000 ) ) ;
#3944 = FACE_OUTER_BOUND ( 'NONE', #109, .T. ) ;
#3945 = PRODUCT_DEFINITION ( 'UNKNOWN', '', #3450, #6065 ) ;
#3946 = AXIS2_PLACEMENT_3D ( 'NONE', #4137, #3403, #6347 ) ;
#3947 = ADVANCED_FACE ( 'NONE', ( #1227 ), #3632, .F. ) ;
#3948 = CARTESIAN_POINT ( 'NONE',  ( -26.02777777777775370, 7.180166011355047395, 0.000000000000000000 ) ) ;
#3949 = CIRCLE ( 'NONE', #4567, 3.000000000000000000 ) ;
#3950 = EDGE_CURVE ( 'NONE', #6722, #4533, #7528, .T. ) ;
#3951 = VERTEX_POINT ( 'NONE', #2733 ) ;
#3952 = VECTOR ( 'NONE', #1786, 1000.000000000000000 ) ;
#3953 = EDGE_CURVE ( 'NONE', #5769, #1000, #3581, .T. ) ;
#3954 = ORIENTED_EDGE ( 'NONE', *, *, #419, .T. ) ;
#3955 = AXIS2_PLACEMENT_3D ( 'NONE', #4575, #7400, #5296 ) ;
#3956 = DIRECTION ( 'NONE',  ( 0.000000000000000000, -0.000000000000000000, 1.000000000000000000 ) ) ;
#3957 = EDGE_CURVE ( 'NONE', #7510, #6770, #7278, .T. ) ;
#3958 = DIRECTION ( 'NONE',  ( -1.000000000000000000, -0.000000000000000000, -0.000000000000000000 ) ) ;
#3959 = VECTOR ( 'NONE', #2055, 1000.000000000000000 ) ;
#3960 = AXIS2_PLACEMENT_3D ( 'NONE', #47, #89, #2242 ) ;
#3961 = CARTESIAN_POINT ( 'NONE',  ( 17.49999999999999645, 4.703319286132082944, 14.49999999999999822 ) ) ;
#3962 = AXIS2_PLACEMENT_3D ( 'NONE', #5776, #6499, #810 ) ;
#3963 = SHAPE_REPRESENTATION ( '1-Center Box', ( #1614 ), #4537 ) ;
#3964 = CARTESIAN_POINT ( 'NONE',  ( 16.50000000000000000, 0.000000000000000000, 5.000000000000000000 ) ) ;
#3965 = VERTEX_POINT ( 'NONE', #2821 ) ;
#3966 = ORIENTED_EDGE ( 'NONE', *, *, #540, .T. ) ;
#3967 = ORIENTED_EDGE ( 'NONE', *, *, #6595, .F. ) ;
#3968 = EDGE_LOOP ( 'NONE', ( #6439, #1064, #4637 ) ) ;
#3969 = CARTESIAN_POINT ( 'NONE',  ( -19.74999999999999645, -43.00000000000000000, -25.00000000000000000 ) ) ;
#3970 = ADVANCED_FACE ( 'NONE', ( #1270 ), #698, .F. ) ;
#3971 = CARTESIAN_POINT ( 'NONE',  ( 0.000000000000000000, -7.653668647301985040, 19.22759065022772873 ) ) ;
#3972 = ADVANCED_FACE ( 'NONE', ( #4310, #2093, #7966, #7233, #6805, #3004 ), #2956, .T. ) ;
#3973 = FACE_OUTER_BOUND ( 'NONE', #3542, .T. ) ;
#3974 = CIRCLE ( 'NONE', #3199, 11.00000000000000000 ) ;
#3975 = EDGE_CURVE ( 'NONE', #7674, #1938, #4154, .T. ) ;
#3976 = CARTESIAN_POINT ( 'NONE',  ( -37.22467645238198486, 47.05659850664388699, -0.5000000000000038858 ) ) ;
#3977 = DIRECTION ( 'NONE',  ( -0.000000000000000000, -0.000000000000000000, -1.000000000000000000 ) ) ;
#3978 = CARTESIAN_POINT ( 'NONE',  ( 2.000000000000000000, 1.673048428422632513E-15, -13.66147716702868031 ) ) ;
#3979 = ORIENTED_EDGE ( 'NONE', *, *, #37, .T. ) ;
#3980 = ORIENTED_EDGE ( 'NONE', *, *, #7826, .T. ) ;
#3981 = DIRECTION ( 'NONE',  ( 1.000000000000000000, 0.000000000000000000, 0.000000000000000000 ) ) ;
#3982 = VECTOR ( 'NONE', #8536, 1000.000000000000000 ) ;
#3983 = VERTEX_POINT ( 'NONE', #6713 ) ;
#3984 = DIRECTION ( 'NONE',  ( 0.000000000000000000, 0.000000000000000000, 1.000000000000000000 ) ) ;
#3985 = VECTOR ( 'NONE', #878, 1000.000000000000000 ) ;
#3986 = DIRECTION ( 'NONE',  ( 0.000000000000000000, 0.000000000000000000, -1.000000000000000000 ) ) ;
#3987 = EDGE_LOOP ( 'NONE', ( #7205, #8456, #1811, #3500 ) ) ;
#3988 = LINE ( 'NONE', #2542, #6572 ) ;
#3989 = DIRECTION ( 'NONE',  ( -0.000000000000000000, -0.000000000000000000, -1.000000000000000000 ) ) ;
#3990 = DIRECTION ( 'NONE',  ( -1.000000000000000000, 0.000000000000000000, 0.000000000000000000 ) ) ;
#3991 = ORIENTED_EDGE ( 'NONE', *, *, #9118, .T. ) ;
#3992 = ORIENTED_EDGE ( 'NONE', *, *, #7174, .F. ) ;
#3993 = ITEM_DEFINED_TRANSFORMATION ( 'NONE', 'NONE', #1465,  #1614 ) ;
#3994 = EDGE_CURVE ( 'NONE', #1000, #1522, #5843, .T. ) ;
#3995 = CARTESIAN_POINT ( 'NONE',  ( 60.00000000000000000, -1.836970198721028011E-15, -85.00000000000000000 ) ) ;
#3996 = DIRECTION ( 'NONE',  ( 1.000000000000000000, -0.000000000000000000, -0.000000000000000000 ) ) ;
#3997 = LINE ( 'NONE', #6165, #2887 ) ;
#3998 = DIRECTION ( 'NONE',  ( 0.000000000000000000, 0.000000000000000000, 1.000000000000000000 ) ) ;
#3999 = FACE_OUTER_BOUND ( 'NONE', #741, .T. ) ;
#4000 = ORIENTED_EDGE ( 'NONE', *, *, #5717, .T. ) ;
#4001 = LINE ( 'NONE', #345, #8850 ) ;
#4002 = ORIENTED_EDGE ( 'NONE', *, *, #8949, .F. ) ;
#4003 = CARTESIAN_POINT ( 'NONE',  ( 37.22467645238198486, -47.05659850664387989, 11.99999999999999645 ) ) ;
#4004 = LINE ( 'NONE', #5448, #6105 ) ;
#4005 = DIRECTION ( 'NONE',  ( -0.000000000000000000, -0.000000000000000000, -1.000000000000000000 ) ) ;
#4006 = EDGE_CURVE ( 'NONE', #2635, #9473, #8867, .T. ) ;
#4007 = CARTESIAN_POINT ( 'NONE',  ( 37.22467645238197775, -47.05659850664388699, -5.608807313787648852 ) ) ;
#4008 = VECTOR ( 'NONE', #5522, 1000.000000000000000 ) ;
#4009 = EDGE_CURVE ( 'NONE', #6154, #1500, #8297, .T. ) ;
#4010 = VERTEX_POINT ( 'NONE', #131 ) ;
#4011 = EDGE_CURVE ( 'NONE', #7415, #975, #7374, .T. ) ;
#4012 = ADVANCED_FACE ( 'NONE', ( #4398 ), #8817, .F. ) ;
#4013 = ORIENTED_EDGE ( 'NONE', *, *, #8984, .F. ) ;
#4014 = EDGE_LOOP ( 'NONE', ( #1223, #5378 ) ) ;
#4015 =( NAMED_UNIT ( * ) SI_UNIT ( $, .STERADIAN. ) SOLID_ANGLE_UNIT ( ) );
#4016 = ORIENTED_EDGE ( 'NONE', *, *, #830, .T. ) ;
#4017 = CARTESIAN_POINT ( 'NONE',  ( 12.37436867076458036, -12.37436867076458036, 19.62563132923542142 ) ) ;
#4018 = CYLINDRICAL_SURFACE ( 'NONE', #3171, 60.00000000000000000 ) ;
#4019 = DIRECTION ( 'NONE',  ( 1.000000000000000000, 0.000000000000000000, 0.000000000000000000 ) ) ;
#4020 = DIRECTION ( 'NONE',  ( 0.000000000000000000, 0.000000000000000000, 1.000000000000000000 ) ) ;
#4021 = FACE_OUTER_BOUND ( 'NONE', #6589, .T. ) ;
#4022 = ORIENTED_EDGE ( 'NONE', *, *, #3530, .T. ) ;
#4023 = EDGE_LOOP ( 'NONE', ( #4648, #614 ) ) ;
#4024 = LINE ( 'NONE', #9103, #4528 ) ;
#4025 = ORIENTED_EDGE ( 'NONE', *, *, #343, .F. ) ;
#4026 = EDGE_CURVE ( 'NONE', #849, #9116, #2006, .T. ) ;
#4027 = CYLINDRICAL_SURFACE ( 'NONE', #5739, 6.000000000000000888 ) ;
#4028 = DIRECTION ( 'NONE',  ( -0.000000000000000000, -0.000000000000000000, -1.000000000000000000 ) ) ;
#4029 = ORIENTED_EDGE ( 'NONE', *, *, #2923, .F. ) ;
#4030 = CIRCLE ( 'NONE', #8617, 11.00000000000000000 ) ;
#4031 = DIRECTION ( 'NONE',  ( 0.000000000000000000, 0.000000000000000000, -1.000000000000000000 ) ) ;
#4032 = EDGE_CURVE ( 'NONE', #5108, #3430, #17, .T. ) ;
#4033 = PLANE ( 'NONE',  #8801 ) ;
#4034 = CARTESIAN_POINT ( 'NONE',  ( 53.29490495164537833, 11.46446609406721961, -97.50000000000002842 ) ) ;
#4035 = VERTEX_POINT ( 'NONE', #3151 ) ;
#4036 = ORIENTED_EDGE ( 'NONE', *, *, #4886, .T. ) ;
#4037 = AXIS2_PLACEMENT_3D ( 'NONE', #4725, #1649, #5356 ) ;
#4038 = DIRECTION ( 'NONE',  ( 1.000000000000000000, 0.000000000000000000, 0.000000000000000000 ) ) ;
#4039 = CARTESIAN_POINT ( 'NONE',  ( -27.00000000000000000, -43.00000000000000000, 11.99999999999999645 ) ) ;
#4040 = DIRECTION ( 'NONE',  ( 1.000000000000000000, 0.000000000000000000, 0.000000000000000000 ) ) ;
#4041 = CARTESIAN_POINT ( 'NONE',  ( 5.000000000000000000, 18.47759065022580316, -7.653668647301631545 ) ) ;
#4042 = VECTOR ( 'NONE', #4786, 1000.000000000000114 ) ;
#4043 = CARTESIAN_POINT ( 'NONE',  ( -19.62310601229373930, 19.62310601229373930, 37.12563132923542497 ) ) ;
#4044 = ADVANCED_FACE ( 'NONE', ( #839 ), #3773, .F. ) ;
#4045 = ORIENTED_EDGE ( 'NONE', *, *, #7665, .T. ) ;
#4046 = DIRECTION ( 'NONE',  ( -0.000000000000000000, -0.000000000000000000, 1.000000000000000000 ) ) ;
#4047 = ORIENTED_EDGE ( 'NONE', *, *, #6576, .T. ) ;
#4048 = FACE_OUTER_BOUND ( 'NONE', #3095, .T. ) ;
#4049 = DIRECTION ( 'NONE',  ( 0.000000000000000000, 0.000000000000000000, -1.000000000000000000 ) ) ;
#4050 = CIRCLE ( 'NONE', #2365, 3.000000000000000000 ) ;
#4051 = EDGE_CURVE ( 'NONE', #4256, #5417, #789, .T. ) ;
#4052 = FACE_OUTER_BOUND ( 'NONE', #681, .T. ) ;
#4053 = LINE ( 'NONE', #6278, #4324 ) ;
#4054 = VECTOR ( 'NONE', #802, 999.9999999999998863 ) ;
#4055 = ORIENTED_EDGE ( 'NONE', *, *, #1713, .F. ) ;
#4056 = ORIENTED_EDGE ( 'NONE', *, *, #6004, .T. ) ;
#4057 = CARTESIAN_POINT ( 'NONE',  ( -56.07586385285964781, 80.45324141007534990, 43.95616229838128675 ) ) ;
#4058 = ORIENTED_EDGE ( 'NONE', *, *, #4113, .F. ) ;
#4059 = CARTESIAN_POINT ( 'NONE',  ( -31.99999999999999289, 0.000000000000000000, 32.00000000000000000 ) ) ;
#4060 = DIRECTION ( 'NONE',  ( 0.000000000000000000, 0.000000000000000000, 1.000000000000000000 ) ) ;
#4061 = AXIS2_PLACEMENT_3D ( 'NONE', #7485, #3303, #3213 ) ;
#4062 = CARTESIAN_POINT ( 'NONE',  ( 4.000000000000000000, -7.653668647301985040, 18.47759065022880520 ) ) ;
#4063 = AXIS2_PLACEMENT_3D ( 'NONE', #4643, #2343, #897 ) ;
#4064 = LINE ( 'NONE', #5606, #5900 ) ;
#4065 = EDGE_LOOP ( 'NONE', ( #7025, #8723, #7925, #6823, #2948, #7979 ) ) ;
#4066 = EDGE_CURVE ( 'NONE', #4647, #4346, #7683, .T. ) ;
#4067 = ORIENTED_EDGE ( 'NONE', *, *, #5113, .F. ) ;
#4068 = PLANE ( 'NONE',  #2092 ) ;
#4069 = ORIENTED_EDGE ( 'NONE', *, *, #2303, .F. ) ;
#4070 = EDGE_CURVE ( 'NONE', #3854, #1904, #9062, .T. ) ;
#4071 = DIRECTION ( 'NONE',  ( 0.000000000000000000, 0.000000000000000000, -1.000000000000000000 ) ) ;
#4072 = CARTESIAN_POINT ( 'NONE',  ( 16.50000000000000000, 0.000000000000000000, 5.000000000000000000 ) ) ;
#4073 = EDGE_LOOP ( 'NONE', ( #3527, #8777, #4435, #647, #7282, #9375 ) ) ;
#4074 = CARTESIAN_POINT ( 'NONE',  ( 0.000000000000000000, 0.000000000000000000, 5.000000000000000000 ) ) ;
#4075 = DIRECTION ( 'NONE',  ( 0.000000000000000000, 0.000000000000000000, -1.000000000000000000 ) ) ;
#4076 = CARTESIAN_POINT ( 'NONE',  ( 0.000000000000000000, 0.000000000000000000, 10.00000000000000000 ) ) ;
#4077 = CARTESIAN_POINT ( 'NONE',  ( -3.000000000000000444, 0.000000000000000000, 20.49999999999999645 ) ) ;
#4078 = CARTESIAN_POINT ( 'NONE',  ( 0.000000000000000000, -17.50000000000000000, 49.50000000000000000 ) ) ;
#4079 = VERTEX_POINT ( 'NONE', #4452 ) ;
#4080 = ORIENTED_EDGE ( 'NONE', *, *, #5238, .T. ) ;
#4081 =( GEOMETRIC_REPRESENTATION_CONTEXT ( 3 ) GLOBAL_UNCERTAINTY_ASSIGNED_CONTEXT ( ( #195 ) ) GLOBAL_UNIT_ASSIGNED_CONTEXT ( ( #6680, #958, #8126 ) ) REPRESENTATION_CONTEXT ( 'NONE', 'WORKASPACE' ) );
#4082 = APPLICATION_PROTOCOL_DEFINITION ( 'draft international standard', 'automotive_design', 1998, #1678 ) ;
#4083 = DIRECTION ( 'NONE',  ( 0.000000000000000000, 0.000000000000000000, 1.000000000000000000 ) ) ;
#4084 = CYLINDRICAL_SURFACE ( 'NONE', #4976, 6.000000000000000888 ) ;
#4085 = CIRCLE ( 'NONE', #8830, 1.560000000002327303 ) ;
#4086 = CYLINDRICAL_SURFACE ( 'NONE', #8412, 3.000000000000002665 ) ;
#4087 = CARTESIAN_POINT ( 'NONE',  ( 5.000000000000000888, 0.000000000000000000, 5.000000000000000000 ) ) ;
#4088 = CARTESIAN_POINT ( 'NONE',  ( 3.499999999999999556, 2.755455298081544778E-15, -22.50000000000000000 ) ) ;
#4089 = ORIENTED_EDGE ( 'NONE', *, *, #7837, .T. ) ;
#4090 = EDGE_LOOP ( 'NONE', ( #3157, #4581, #911, #9342 ) ) ;
#4091 = VECTOR ( 'NONE', #2527, 1000.000000000000114 ) ;
#4092 = LINE ( 'NONE', #7070, #8320 ) ;
#4093 = AXIS2_PLACEMENT_3D ( 'NONE', #4116, #7857, #6331 ) ;
#4094 = DIRECTION ( 'NONE',  ( 1.000000000000000000, 0.000000000000000000, 0.000000000000000000 ) ) ;
#4095 = DIRECTION ( 'NONE',  ( -1.000000000000000000, 0.000000000000000000, 0.000000000000000000 ) ) ;
#4096 = DIRECTION ( 'NONE',  ( -0.000000000000000000, -0.000000000000000000, -1.000000000000000000 ) ) ;
#4097 = VECTOR ( 'NONE', #6026, 1000.000000000000000 ) ;
#4098 = DIRECTION ( 'NONE',  ( 0.000000000000000000, 0.3976074376343005090, -0.9175556253099241832 ) ) ;
#4099 = CIRCLE ( 'NONE', #7316, 13.50000000000000178 ) ;
#4100 = VERTEX_POINT ( 'NONE', #7469 ) ;
#4101 = ORIENTED_EDGE ( 'NONE', *, *, #3002, .T. ) ;
#4102 = CARTESIAN_POINT ( 'NONE',  ( 70.51394605043111596, 96.36314398677507143, 28.04625972168022230 ) ) ;
#4103 = ORIENTED_EDGE ( 'NONE', *, *, #7618, .T. ) ;
#4104 = AXIS2_PLACEMENT_3D ( 'NONE', #7247, #667, #5811 ) ;
#4105 = FACE_BOUND ( 'NONE', #8366, .T. ) ;
#4106 = TOROIDAL_SURFACE ( 'NONE', #7637, 15.66147716702868209, 2.000000000000000000 ) ;
#4107 = FACE_OUTER_BOUND ( 'NONE', #1861, .T. ) ;
#4108 = CIRCLE ( 'NONE', #6881, 8.000000000000021316 ) ;
#4109 = DIRECTION ( 'NONE',  ( 1.000000000000000000, 0.000000000000000000, 0.000000000000000000 ) ) ;
#4110 = CIRCLE ( 'NONE', #3647, 0.7500000000013675727 ) ;
#4111 = LINE ( 'NONE', #456, #3594 ) ;
#4112 = DIRECTION ( 'NONE',  ( 1.000000000000000000, 0.000000000000000000, 0.000000000000000000 ) ) ;
#4113 = EDGE_CURVE ( 'NONE', #3384, #6270, #896, .T. ) ;
#4114 = ORIENTED_EDGE ( 'NONE', *, *, #3140, .T. ) ;
#4115 = ORIENTED_EDGE ( 'NONE', *, *, #6949, .T. ) ;
#4116 = CARTESIAN_POINT ( 'NONE',  ( 22.50000000000000355, 2.356749903719115078E-13, 15.00000000000000000 ) ) ;
#4117 = ORIENTED_EDGE ( 'NONE', *, *, #4439, .F. ) ;
#4118 = CARTESIAN_POINT ( 'NONE',  ( 26.21170834203226718, -53.97171801779368394, -2.612255525622730001 ) ) ;
#4119 = DIRECTION ( 'NONE',  ( -1.000000000000000000, -0.000000000000000000, -0.000000000000000000 ) ) ;
#4120 = VECTOR ( 'NONE', #4928, 1000.000000000000000 ) ;
#4121 = ORIENTED_EDGE ( 'NONE', *, *, #713, .F. ) ;
#4122 = FACE_OUTER_BOUND ( 'NONE', #2240, .T. ) ;
#4123 = CARTESIAN_POINT ( 'NONE',  ( -0.7500000000000000000, -2.749999999999995559, 1.500000000000000000 ) ) ;
#4124 = EDGE_CURVE ( 'NONE', #458, #1534, #749, .T. ) ;
#4125 = DIRECTION ( 'NONE',  ( 0.000000000000000000, 0.000000000000000000, -1.000000000000000000 ) ) ;
#4126 = CIRCLE ( 'NONE', #3207, 0.7499999999989250821 ) ;
#4127 = CARTESIAN_POINT ( 'NONE',  ( 28.48725673979378570, 2.337639529181963827, 1.581093618438869086 ) ) ;
#4128 = EDGE_CURVE ( 'NONE', #5535, #4476, #4615, .T. ) ;
#4129 = ORIENTED_EDGE ( 'NONE', *, *, #4168, .T. ) ;
#4130 = ORIENTED_EDGE ( 'NONE', *, *, #4597, .T. ) ;
#4131 = EDGE_CURVE ( 'NONE', #3545, #2406, #6089, .T. ) ;
#4132 = ADVANCED_FACE ( 'NONE', ( #8440 ), #8291, .T. ) ;
#4133 = APPLICATION_CONTEXT ( 'automotive_design' ) ;
#4134 = SHAPE_DEFINITION_REPRESENTATION ( #7302, #6298 ) ;
#4135 = LINE ( 'NONE', #6446, #7433 ) ;
#4136 = DIRECTION ( 'NONE',  ( -1.000000000000000000, 0.000000000000000000, 0.000000000000000000 ) ) ;
#4137 = CARTESIAN_POINT ( 'NONE',  ( 0.000000000000000000, 0.000000000000000000, 21.00000000000000000 ) ) ;
#4138 = ORIENTED_EDGE ( 'NONE', *, *, #4994, .T. ) ;
#4139 = EDGE_CURVE ( 'NONE', #4458, #7922, #8599, .T. ) ;
#4140 = VERTEX_POINT ( 'NONE', #7758 ) ;
#4141 = ORIENTED_EDGE ( 'NONE', *, *, #9442, .F. ) ;
#4142 = EDGE_CURVE ( 'NONE', #3455, #4158, #1854, .T. ) ;
#4143 = DIRECTION ( 'NONE',  ( 1.000000000000000000, 0.000000000000000000, 0.000000000000000000 ) ) ;
#4144 = CARTESIAN_POINT ( 'NONE',  ( -27.00000000000000000, 43.00000000000000000, 11.99999999999999645 ) ) ;
#4145 = DIRECTION ( 'NONE',  ( 1.000000000000000000, 0.000000000000000000, 0.000000000000000000 ) ) ;
#4146 = DIRECTION ( 'NONE',  ( -0.000000000000000000, -0.000000000000000000, -1.000000000000000000 ) ) ;
#4147 = FACE_OUTER_BOUND ( 'NONE', #5628, .T. ) ;
#4148 = ORIENTED_EDGE ( 'NONE', *, *, #7924, .T. ) ;
#4149 = VERTEX_POINT ( 'NONE', #3338 ) ;
#4150 =( LENGTH_UNIT ( ) NAMED_UNIT ( * ) SI_UNIT ( .MILLI., .METRE. ) );
#4151 = EDGE_LOOP ( 'NONE', ( #4393, #5950, #8893, #7944 ) ) ;
#4152 = CARTESIAN_POINT ( 'NONE',  ( 4.000000000000000000, 6.938893903907240211E-16, 0.000000000000000000 ) ) ;
#4153 = CARTESIAN_POINT ( 'NONE',  ( -31.99999999999999289, 35.00000000000000000, 5.000000000000004441 ) ) ;
#4154 = CIRCLE ( 'NONE', #3233, 15.00000000000000000 ) ;
#4155 = CARTESIAN_POINT ( 'NONE',  ( 38.00000000000000000, 44.39318849903271769, -6.762951650419155136 ) ) ;
#4156 = PLANE ( 'NONE',  #4207 ) ;
#4157 = FACE_OUTER_BOUND ( 'NONE', #2762, .T. ) ;
#4158 = VERTEX_POINT ( 'NONE', #6946 ) ;
#4159 = VERTEX_POINT ( 'NONE', #1897 ) ;
#4160 = CARTESIAN_POINT ( 'NONE',  ( -15.99999999999999289, 20.99999999999999289, -16.89999999999999858 ) ) ;
#4161 = VECTOR ( 'NONE', #6558, 1000.000000000000227 ) ;
#4162 = EDGE_LOOP ( 'NONE', ( #7799, #9153, #1844, #3902 ) ) ;
#4163 = EDGE_CURVE ( 'NONE', #5672, #8983, #1544, .T. ) ;
#4164 = DIRECTION ( 'NONE',  ( -0.000000000000000000, -0.000000000000000000, 1.000000000000000000 ) ) ;
#4165 = CARTESIAN_POINT ( 'NONE',  ( 27.00000000000000000, -43.00000000000000000, 25.00000000000000000 ) ) ;
#4166 = DIRECTION ( 'NONE',  ( 0.000000000000000000, 0.000000000000000000, 1.000000000000000000 ) ) ;
#4167 = DIRECTION ( 'NONE',  ( 1.000000000000000000, 0.000000000000000000, -0.000000000000000000 ) ) ;
#4168 = EDGE_CURVE ( 'NONE', #7251, #1024, #7991, .T. ) ;
#4169 = CARTESIAN_POINT ( 'NONE',  ( 4.000000000000000888, 0.000000000000000000, 17.50000000000000000 ) ) ;
#4170 = CARTESIAN_POINT ( 'NONE',  ( 28.61681370049857875, 1.683481704175382010, 1.664380236034806337 ) ) ;
#4171 = ORIENTED_EDGE ( 'NONE', *, *, #8162, .F. ) ;
#4172 = ORIENTED_EDGE ( 'NONE', *, *, #2719, .F. ) ;
#4173 = CONICAL_SURFACE ( 'NONE', #39, 18.50000000000001776, 0.7853981633974431720 ) ;
#4174 = ITEM_DEFINED_TRANSFORMATION ( 'NONE', 'NONE', #248,  #1614 ) ;
#4175 = CARTESIAN_POINT ( 'NONE',  ( 27.00000000000000355, 35.00000000000000000, 5.000000000000004441 ) ) ;
#4176 = CARTESIAN_POINT ( 'NONE',  ( 12.37436867076458036, 12.37436867076458036, 19.62563132923542142 ) ) ;
#4177 = LINE ( 'NONE', #1284, #8088 ) ;
#4178 = ORIENTED_EDGE ( 'NONE', *, *, #6729, .F. ) ;
#4179 = ORIENTED_EDGE ( 'NONE', *, *, #2848, .T. ) ;
#4180 = CONICAL_SURFACE ( 'NONE', #2505, 22.00000000000000711, 0.7853981633974482790 ) ;
#4181 = ORIENTED_EDGE ( 'NONE', *, *, #488, .F. ) ;
#4182 = VERTEX_POINT ( 'NONE', #1708 ) ;
#4183 = EDGE_CURVE ( 'NONE', #3097, #4382, #359, .T. ) ;
#4184 = PLANE ( 'NONE',  #2950 ) ;
#4185 = CARTESIAN_POINT ( 'NONE',  ( -15.99999999999999645, -43.00000000000000000, -7.366666666666667140 ) ) ;
#4186 = TOROIDAL_SURFACE ( 'NONE', #6495, 16.00000000000000000, 1.000000000000000000 ) ;
#4187 = CARTESIAN_POINT ( 'NONE',  ( -53.29490495164537833, -15.90990257669733943, -85.90990257669729147 ) ) ;
#4188 = DIRECTION ( 'NONE',  ( 0.000000000000000000, 0.000000000000000000, 1.000000000000000000 ) ) ;
#4189 = FACE_BOUND ( 'NONE', #5493, .T. ) ;
#4190 = ORIENTED_EDGE ( 'NONE', *, *, #8035, .T. ) ;
#4191 = ORIENTED_EDGE ( 'NONE', *, *, #1126, .F. ) ;
#4192 = SHAPE_REPRESENTATION_RELATIONSHIP ( 'NONE' , 'NONE' ,  #3963, #5431 ) ;
#4193 = EDGE_LOOP ( 'NONE', ( #1763, #5432, #3804, #5728 ) ) ;
#4194 = CARTESIAN_POINT ( 'NONE',  ( 27.00000000000000355, -34.99999999999999289, 5.000000000000004441 ) ) ;
#4195 = AXIS2_PLACEMENT_3D ( 'NONE', #8221, #8719, #5066 ) ;
#4196 = LINE ( 'NONE', #4153, #8545 ) ;
#4197 = DIRECTION ( 'NONE',  ( -0.000000000000000000, -0.000000000000000000, -1.000000000000000000 ) ) ;
#4198 = CARTESIAN_POINT ( 'NONE',  ( -53.29490495164537833, 15.90990257669733943, -54.09009742330271564 ) ) ;
#4199 = DIRECTION ( 'NONE',  ( 0.000000000000000000, 0.000000000000000000, 1.000000000000000000 ) ) ;
#4200 = ORIENTED_EDGE ( 'NONE', *, *, #251, .F. ) ;
#4201 = VERTEX_POINT ( 'NONE', #7042 ) ;
#4202 = LINE ( 'NONE', #7956, #1945 ) ;
#4203 = EDGE_LOOP ( 'NONE', ( #3790, #1547, #7369, #1460 ) ) ;
#4204 = DIRECTION ( 'NONE',  ( -1.000000000000000000, 0.000000000000000000, 0.000000000000000000 ) ) ;
#4205 = DIRECTION ( 'NONE',  ( 1.224646799147353207E-16, 1.000000000000000000, -0.000000000000000000 ) ) ;
#4206 = LINE ( 'NONE', #8584, #8539 ) ;
#4207 = AXIS2_PLACEMENT_3D ( 'NONE', #7716, #3289, #274 ) ;
#4208 = LINE ( 'NONE', #4930, #5997 ) ;
#4209 = EDGE_CURVE ( 'NONE', #2688, #3554, #1860, .T. ) ;
#4210 = DIRECTION ( 'NONE',  ( 0.000000000000000000, 0.000000000000000000, -1.000000000000000000 ) ) ;
#4211 = CARTESIAN_POINT ( 'NONE',  ( 28.75000000000003553, 0.3373484206894367676, 1.750000000000026423 ) ) ;
#4212 = ORIENTED_EDGE ( 'NONE', *, *, #7704, .F. ) ;
#4213 = AXIS2_PLACEMENT_3D ( 'NONE', #3173, #7496, #9076 ) ;
#4214 = ORIENTED_EDGE ( 'NONE', *, *, #6950, .T. ) ;
#4215 = DIRECTION ( 'NONE',  ( -1.000000000000000000, -0.000000000000000000, -0.000000000000000000 ) ) ;
#4216 = EDGE_CURVE ( 'NONE', #8987, #7578, #3381, .T. ) ;
#4217 = CONTEXT_DEPENDENT_SHAPE_REPRESENTATION ( #8846, #7459 ) ;
#4218 = DIRECTION ( 'NONE',  ( -1.000000000000000000, 0.000000000000000000, -0.000000000000000000 ) ) ;
#4219 = DIRECTION ( 'NONE',  ( -1.000000000000000000, 0.000000000000000000, 0.000000000000000000 ) ) ;
#4220 = CARTESIAN_POINT ( 'NONE',  ( 50.79490495164537833, 12.50000000000000000, -100.0000000000000000 ) ) ;
#4221 = DIRECTION ( 'NONE',  ( -1.000000000000000000, 0.000000000000000000, 0.000000000000000000 ) ) ;
#4222 = AXIS2_PLACEMENT_3D ( 'NONE', #492, #9327, #2621 ) ;
#4223 = VERTEX_POINT ( 'NONE', #3244 ) ;
#4224 = ORIENTED_EDGE ( 'NONE', *, *, #6027, .T. ) ;
#4225 = EDGE_CURVE ( 'NONE', #5660, #3926, #1706, .T. ) ;
#4226 = ORIENTED_EDGE ( 'NONE', *, *, #4882, .T. ) ;
#4227 = ORIENTED_EDGE ( 'NONE', *, *, #1362, .T. ) ;
#4228 = CARTESIAN_POINT ( 'NONE',  ( 0.000000000000000000, 0.000000000000000000, 23.99999999999998579 ) ) ;
#4229 = CARTESIAN_POINT ( 'NONE',  ( 6.000000000000157208, -22.50000000000000355, 0.000000000000000000 ) ) ;
#4230 = PRODUCT_DEFINITION_SHAPE ( 'NONE', 'NONE',  #9479 ) ;
#4231 = CARTESIAN_POINT ( 'NONE',  ( 32.00000000000000711, 29.99999999999997868, 58.99999999999997158 ) ) ;
#4232 = EDGE_CURVE ( 'NONE', #3144, #2690, #7715, .T. ) ;
#4233 = EDGE_CURVE ( 'NONE', #8754, #3144, #7670, .T. ) ;
#4234 = CARTESIAN_POINT ( 'NONE',  ( 34.25000000000000000, -43.00000000000000000, 25.00000000000000000 ) ) ;
#4235 = EDGE_LOOP ( 'NONE', ( #5851, #7913 ) ) ;
#4236 = VECTOR ( 'NONE', #3519, 1000.000000000000000 ) ;
#4237 = PLANE ( 'NONE',  #5632 ) ;
#4238 = EDGE_CURVE ( 'NONE', #883, #5050, #5849, .T. ) ;
#4239 = EDGE_CURVE ( 'NONE', #794, #3697, #2321, .T. ) ;
#4240 = ORIENTED_EDGE ( 'NONE', *, *, #4239, .F. ) ;
#4241 = CARTESIAN_POINT ( 'NONE',  ( -50.79490495164537833, -30.00000000000000000, -100.0000000000000000 ) ) ;
#4242 = CARTESIAN_POINT ( 'NONE',  ( 38.00000000000000000, 43.00000000000000000, -7.366666666666667140 ) ) ;
#4243 = CARTESIAN_POINT ( 'NONE',  ( 4.000000000000000000, 14.14213562373247868, 15.70213562373191962 ) ) ;
#4244 = AXIS2_PLACEMENT_3D ( 'NONE', #6557, #5925, #2989 ) ;
#4245 = EDGE_CURVE ( 'NONE', #6044, #5505, #4825, .T. ) ;
#4246 = DIRECTION ( 'NONE',  ( 0.000000000000000000, 0.000000000000000000, 1.000000000000000000 ) ) ;
#4247 =( REPRESENTATION_RELATIONSHIP ('NONE','NONE', #1933, #8501 ) REPRESENTATION_RELATIONSHIP_WITH_TRANSFORMATION ( #9253 )SHAPE_REPRESENTATION_RELATIONSHIP( ) );
#4248 = CONICAL_SURFACE ( 'NONE', #4563, 14.49999999999998401, 0.7853981633974533860 ) ;
#4249 = DIRECTION ( 'NONE',  ( -1.000000000000000000, 0.000000000000000000, 0.000000000000000000 ) ) ;
#4250 = EDGE_LOOP ( 'NONE', ( #1737, #6781, #5977, #995 ) ) ;
#4251 = AXIS2_PLACEMENT_3D ( 'NONE', #715, #3649, #6586 ) ;
#4252 = EDGE_CURVE ( 'NONE', #955, #2481, #2579, .T. ) ;
#4253 = ORIENTED_EDGE ( 'NONE', *, *, #4715, .T. ) ;
#4254 = LINE ( 'NONE', #7766, #3321 ) ;
#4255 = AXIS2_PLACEMENT_3D ( 'NONE', #795, #8158, #7428 ) ;
#4256 = VERTEX_POINT ( 'NONE', #6187 ) ;
#4257 = EDGE_CURVE ( 'NONE', #5515, #6613, #2927, .T. ) ;
#4258 = CONICAL_SURFACE ( 'NONE', #3026, 28.00000000000000711, 0.7853981633974473908 ) ;
#4259 = FACE_OUTER_BOUND ( 'NONE', #5873, .T. ) ;
#4260 = CARTESIAN_POINT ( 'NONE',  ( 14.49999999999998401, 1.775737858763660240E-15, 27.50000000000000355 ) ) ;
#4261 = EDGE_CURVE ( 'NONE', #9251, #4913, #2529, .T. ) ;
#4262 = DIRECTION ( 'NONE',  ( -0.000000000000000000, -0.000000000000000000, 1.000000000000000000 ) ) ;
#4263 = CIRCLE ( 'NONE', #6116, 2.999999999999999556 ) ;
#4264 = DIRECTION ( 'NONE',  ( -1.000000000000000000, 0.000000000000000000, 0.000000000000000000 ) ) ;
#4265 = VECTOR ( 'NONE', #7732, 1000.000000000000000 ) ;
#4266 = AXIS2_PLACEMENT_3D ( 'NONE', #1058, #9119, #5480 ) ;
#4267 =( BOUNDED_CURVE ( )  B_SPLINE_CURVE ( 3, ( #8015, #6532, #2969, #6584 ),
 .UNSPECIFIED., .F., .T. ) 
 B_SPLINE_CURVE_WITH_KNOTS ( ( 4, 4 ),
 ( 1.570796326794896558, 1.948494305174372832 ),
 .UNSPECIFIED. ) 
 CURVE ( )  GEOMETRIC_REPRESENTATION_ITEM ( )  RATIONAL_B_SPLINE_CURVE ( ( 1.000000000000000000, 0.9881473088045071851, 0.9881473088045071851, 1.000000000000000000 ) ) 
 REPRESENTATION_ITEM ( '' )  );
#4268 = CARTESIAN_POINT ( 'NONE',  ( -72.75414293302374347, 30.00000000000000000, -51.44494782735612404 ) ) ;
#4269 = CARTESIAN_POINT ( 'NONE',  ( -25.50000000000000355, 0.000000000000000000, 5.000000000000000000 ) ) ;
#4270 = ORIENTED_EDGE ( 'NONE', *, *, #6007, .T. ) ;
#4271 = VERTEX_POINT ( 'NONE', #8384 ) ;
#4272 = CIRCLE ( 'NONE', #5652, 6.000000000000001776 ) ;
#4273 = LINE ( 'NONE', #2512, #2103 ) ;
#4274 = CARTESIAN_POINT ( 'NONE',  ( -22.50000000000000355, 0.000000000000000000, 2.000000000000039080 ) ) ;
#4275 = VECTOR ( 'NONE', #2229, 1000.000000000000114 ) ;
#4276 = AXIS2_PLACEMENT_3D ( 'NONE', #6742, #725, #1394 ) ;
#4277 = CARTESIAN_POINT ( 'NONE',  ( 17.50000000000000355, 0.000000000000000000, 14.49999999999999822 ) ) ;
#4278 = DIRECTION ( 'NONE',  ( -0.5773502691896290617, -0.5773502691896258421, 0.5773502691896225114 ) ) ;
#4279 = ORIENTED_EDGE ( 'NONE', *, *, #3292, .F. ) ;
#4280 = EDGE_LOOP ( 'NONE', ( #1213, #7606, #1879, #5006 ) ) ;
#4281 = ORIENTED_EDGE ( 'NONE', *, *, #104, .T. ) ;
#4282 = CIRCLE ( 'NONE', #1297, 18.50000000000001776 ) ;
#4283 = ORIENTED_EDGE ( 'NONE', *, *, #3281, .T. ) ;
#4284 = CONICAL_SURFACE ( 'NONE', #6583, 22.50000000000000000, 0.7853981633974447263 ) ;
#4285 = CARTESIAN_POINT ( 'NONE',  ( 28.13653351783517209, -2.066994717595015629, 1.211640400093609848 ) ) ;
#4286 = CARTESIAN_POINT ( 'NONE',  ( 37.00000000000000711, -30.00000000000000000, -13.00000000000000000 ) ) ;
#4287 = DIRECTION ( 'NONE',  ( -0.2588190451025176309, 0.000000000000000000, -0.9659258262890692004 ) ) ;
#4288 = CARTESIAN_POINT ( 'NONE',  ( 2.000000000000000000, 0.000000000000000000, 0.000000000000000000 ) ) ;
#4289 = LINE ( 'NONE', #3563, #6714 ) ;
#4290 = VERTEX_POINT ( 'NONE', #4741 ) ;
#4291 = CARTESIAN_POINT ( 'NONE',  ( -15.70011763207404876, 9.048619709455115512, 16.29988236792595302 ) ) ;
#4292 = ORIENTED_EDGE ( 'NONE', *, *, #4245, .T. ) ;
#4293 = DIRECTION ( 'NONE',  ( -1.000000000000000000, 0.000000000000000000, 0.000000000000000000 ) ) ;
#4294 = EDGE_CURVE ( 'NONE', #4348, #5740, #5510, .T. ) ;
#4295 = CIRCLE ( 'NONE', #8728, 30.00000000000000000 ) ;
#4296 = CARTESIAN_POINT ( 'NONE',  ( 0.000000000000000000, 0.000000000000000000, 11.99999999999999645 ) ) ;
#4297 = EDGE_CURVE ( 'NONE', #6389, #7685, #2768, .T. ) ;
#4298 = DIRECTION ( 'NONE',  ( 0.000000000000000000, 0.7071067811865493491, -0.7071067811865456854 ) ) ;
#4299 = EDGE_CURVE ( 'NONE', #8200, #2677, #6468, .T. ) ;
#4300 = EDGE_CURVE ( 'NONE', #9426, #3888, #3618, .T. ) ;
#4301 = CARTESIAN_POINT ( 'NONE',  ( 22.50000000000000355, 0.000000000000000000, 10.00000000000000000 ) ) ;
#4302 = EDGE_LOOP ( 'NONE', ( #7977, #3992 ) ) ;
#4303 = EDGE_LOOP ( 'NONE', ( #1345, #7559, #8807, #6646 ) ) ;
#4304 = SURFACE_STYLE_USAGE ( .BOTH. , #6658 ) ;
#4305 = EDGE_LOOP ( 'NONE', ( #2632, #7489 ) ) ;
#4306 = DIRECTION ( 'NONE',  ( 1.000000000000000000, 0.000000000000000000, 0.000000000000000000 ) ) ;
#4307 = CARTESIAN_POINT ( 'NONE',  ( -26.64999999999995950, -4.333301281932866900, 0.000000000000000000 ) ) ;
#4308 = AXIS2_PLACEMENT_3D ( 'NONE', #4977, #5846, #4167 ) ;
#4309 = DIRECTION ( 'NONE',  ( 0.000000000000000000, 0.000000000000000000, 1.000000000000000000 ) ) ;
#4310 = FACE_BOUND ( 'NONE', #188, .T. ) ;
#4311 = CARTESIAN_POINT ( 'NONE',  ( -26.99999999999998934, 35.00000000000000000, 5.000000000000004441 ) ) ;
#4312 = VECTOR ( 'NONE', #2856, 1000.000000000000000 ) ;
#4313 = FACE_OUTER_BOUND ( 'NONE', #6485, .T. ) ;
#4314 = EDGE_CURVE ( 'NONE', #7012, #9473, #8615, .T. ) ;
#4315 = ORIENTED_EDGE ( 'NONE', *, *, #8741, .T. ) ;
#4316 = VERTEX_POINT ( 'NONE', #6509 ) ;
#4317 = DIRECTION ( 'NONE',  ( 0.000000000000000000, 0.000000000000000000, 1.000000000000000000 ) ) ;
#4318 = PRODUCT_DEFINITION_SHAPE ( 'NONE', 'NONE',  #9485 ) ;
#4319 = EDGE_CURVE ( 'NONE', #3951, #3236, #4776, .T. ) ;
#4320 = FACE_OUTER_BOUND ( 'NONE', #8125, .T. ) ;
#4321 =( BOUNDED_CURVE ( )  B_SPLINE_CURVE ( 3, ( #6354, #2701, #7207, #4185 ),
 .UNSPECIFIED., .F., .T. ) 
 B_SPLINE_CURVE_WITH_KNOTS ( ( 4, 4 ),
 ( 4.712388980384689674, 7.853981633974482790 ),
 .UNSPECIFIED. ) 
 CURVE ( )  GEOMETRIC_REPRESENTATION_ITEM ( )  RATIONAL_B_SPLINE_CURVE ( ( 1.000000000000000000, 0.3333333333333333703, 0.3333333333333333703, 1.000000000000000000 ) ) 
 REPRESENTATION_ITEM ( '' )  );
#4322 = FACE_OUTER_BOUND ( 'NONE', #3968, .T. ) ;
#4323 = CARTESIAN_POINT ( 'NONE',  ( -25.50000000000000355, 0.000000000000000000, 10.00000000000000000 ) ) ;
#4324 = VECTOR ( 'NONE', #6219, 1000.000000000000000 ) ;
#4325 = ORIENTED_EDGE ( 'NONE', *, *, #3653, .F. ) ;
#4326 = ORIENTED_EDGE ( 'NONE', *, *, #6652, .T. ) ;
#4327 = ORIENTED_EDGE ( 'NONE', *, *, #7153, .T. ) ;
#4328 = ORIENTED_EDGE ( 'NONE', *, *, #3412, .T. ) ;
#4329 = CYLINDRICAL_SURFACE ( 'NONE', #3312, 3.000000000000002665 ) ;
#4330 = CIRCLE ( 'NONE', #5570, 2.999999999999999112 ) ;
#4331 = FACE_OUTER_BOUND ( 'NONE', #5514, .T. ) ;
#4332 = DIRECTION ( 'NONE',  ( -1.000000000000000000, 0.000000000000000000, 0.000000000000000000 ) ) ;
#4333 = CARTESIAN_POINT ( 'NONE',  ( -28.61681370049858231, -1.683481704175391780, 1.664380236034809890 ) ) ;
#4334 = AXIS2_PLACEMENT_3D ( 'NONE', #443, #4143, #9220 ) ;
#4335 = EDGE_CURVE ( 'NONE', #4745, #5080, #7806, .T. ) ;
#4336 = FACE_BOUND ( 'NONE', #526, .T. ) ;
#4337 = ORIENTED_EDGE ( 'NONE', *, *, #2121, .T. ) ;
#4338 = CYLINDRICAL_SURFACE ( 'NONE', #2715, 11.00000000000000000 ) ;
#4339 = VERTEX_POINT ( 'NONE', #7992 ) ;
#4340 = FACE_BOUND ( 'NONE', #4023, .T. ) ;
#4341 = ADVANCED_FACE ( 'NONE', ( #2716 ), #4872, .T. ) ;
#4342 = CARTESIAN_POINT ( 'NONE',  ( 0.000000000000000000, 22.50000000000000355, 10.00000000000000000 ) ) ;
#4343 = DIRECTION ( 'NONE',  ( -1.000000000000000000, 0.000000000000000000, 0.000000000000000000 ) ) ;
#4344 = CARTESIAN_POINT ( 'NONE',  ( 32.00000000000000711, 0.000000000000000000, 13.49999999999999822 ) ) ;
#4345 = CARTESIAN_POINT ( 'NONE',  ( 1.691658612279592466, -28.27209108258186276, 1.319590333518659397 ) ) ;
#4346 = VERTEX_POINT ( 'NONE', #3570 ) ;
#4347 = VECTOR ( 'NONE', #4249, 1000.000000000000000 ) ;
#4348 = VERTEX_POINT ( 'NONE', #4243 ) ;
#4349 = CARTESIAN_POINT ( 'NONE',  ( 0.8460976106428692578, 28.45495154861555420, 1.464499174736009879 ) ) ;
#4350 = EDGE_LOOP ( 'NONE', ( #9228, #3573 ) ) ;
#4351 = CARTESIAN_POINT ( 'NONE',  ( -27.61161645726460989, -3.165483362335529183, 0.7903941804162353257 ) ) ;
#4352 = DIRECTION ( 'NONE',  ( -1.000000000000000000, 0.000000000000000000, 0.000000000000000000 ) ) ;
#4353 = CARTESIAN_POINT ( 'NONE',  ( 0.000000000000000000, 0.000000000000000000, 17.50000000000000000 ) ) ;
#4354 = CARTESIAN_POINT ( 'NONE',  ( -27.00000000000000000, -43.00000000000000000, 11.99999999999999645 ) ) ;
#4355 = AXIS2_PLACEMENT_3D ( 'NONE', #7854, #2721, #5561 ) ;
#4356 = PRODUCT_RELATED_PRODUCT_CATEGORY ( 'part', '', ( #5082 ) ) ;
#4357 = EDGE_CURVE ( 'NONE', #5609, #5683, #1389, .T. ) ;
#4358 = DIRECTION ( 'NONE',  ( -0.000000000000000000, 1.000000000000000000, -0.000000000000000000 ) ) ;
#4359 = CARTESIAN_POINT ( 'NONE',  ( 0.000000000000000000, 0.000000000000000000, 0.000000000000000000 ) ) ;
#4360 = ADVANCED_FACE ( 'NONE', ( #2038 ), #3427, .F. ) ;
#4361 = ORIENTED_EDGE ( 'NONE', *, *, #9287, .F. ) ;
#4362 = AXIS2_PLACEMENT_3D ( 'NONE', #3072, #91, #3017 ) ;
#4363 = VERTEX_POINT ( 'NONE', #4965 ) ;
#4364 = CARTESIAN_POINT ( 'NONE',  ( 0.000000000000000000, -22.50000000000000355, 5.000000000000000000 ) ) ;
#4365 = CARTESIAN_POINT ( 'NONE',  ( -50.79490495164537833, 29.99999999999999645, -82.50000000000000000 ) ) ;
#4366 = VECTOR ( 'NONE', #6318, 1000.000000000000000 ) ;
#4367 = DIRECTION ( 'NONE',  ( -0.000000000000000000, 1.000000000000000000, -0.000000000000000000 ) ) ;
#4368 = DIRECTION ( 'NONE',  ( 0.000000000000000000, 0.000000000000000000, 1.000000000000000000 ) ) ;
#4369 = ORIENTED_EDGE ( 'NONE', *, *, #8062, .F. ) ;
#4370 = ORIENTED_EDGE ( 'NONE', *, *, #6377, .T. ) ;
#4371 = ORIENTED_EDGE ( 'NONE', *, *, #6356, .T. ) ;
#4372 = DIRECTION ( 'NONE',  ( 0.000000000000000000, 0.9997175446104180629, -0.02376617340079609578 ) ) ;
#4373 = ORIENTED_EDGE ( 'NONE', *, *, #5942, .F. ) ;
#4374 = CARTESIAN_POINT ( 'NONE',  ( 60.00000000000000000, -15.90990257669733943, -88.90990257669730568 ) ) ;
#4375 = CARTESIAN_POINT ( 'NONE',  ( 53.29490495164537833, 27.56180520566615044, -81.40266088840108694 ) ) ;
#4376 = CARTESIAN_POINT ( 'NONE',  ( 5.000000000000000000, -7.653668647303860872, -17.72759065022311731 ) ) ;
#4377 = CARTESIAN_POINT ( 'NONE',  ( -22.50000000000000000, -7.855833012397050680E-14, 5.000000000000000000 ) ) ;
#4378 = FACE_OUTER_BOUND ( 'NONE', #5477, .T. ) ;
#4379 = DIRECTION ( 'NONE',  ( -1.000000000000000000, 0.000000000000000000, -0.000000000000000000 ) ) ;
#4380 = VERTEX_POINT ( 'NONE', #2081 ) ;
#4381 = CARTESIAN_POINT ( 'NONE',  ( 16.00000000000000000, 49.08300322764475254, -4.730698601353941157 ) ) ;
#4382 = VERTEX_POINT ( 'NONE', #7173 ) ;
#4383 = AXIS2_PLACEMENT_3D ( 'NONE', #6590, #9274, #8568 ) ;
#4384 = FACE_OUTER_BOUND ( 'NONE', #4553, .T. ) ;
#4385 = LINE ( 'NONE', #4441, #4097 ) ;
#4386 = CARTESIAN_POINT ( 'NONE',  ( -4.333301281932778082, 26.64999999999997371, 0.000000000000000000 ) ) ;
#4387 = CYLINDRICAL_SURFACE ( 'NONE', #9378, 17.50000000000000355 ) ;
#4388 = CIRCLE ( 'NONE', #8988, 15.00000000000000000 ) ;
#4389 = PRODUCT_DEFINITION_SHAPE ( 'NONE', 'NONE',  #9492 ) ;
#4390 = ORIENTED_EDGE ( 'NONE', *, *, #8637, .T. ) ;
#4391 = ORIENTED_EDGE ( 'NONE', *, *, #8852, .T. ) ;
#4392 = CARTESIAN_POINT ( 'NONE',  ( 1.571166602479410136E-13, -22.50000000000000355, 5.000000000000000000 ) ) ;
#4393 = ORIENTED_EDGE ( 'NONE', *, *, #7358, .F. ) ;
#4394 = CARTESIAN_POINT ( 'NONE',  ( 4.000000000000000000, -20.00000000000120437, 2.661998082081668380E-12 ) ) ;
#4395 = VECTOR ( 'NONE', #2126, 999.9999999999998863 ) ;
#4396 = DIRECTION ( 'NONE',  ( 0.000000000000000000, 0.7071067811865473507, 0.7071067811865477948 ) ) ;
#4397 = VECTOR ( 'NONE', #8865, 1000.000000000000000 ) ;
#4398 = FACE_OUTER_BOUND ( 'NONE', #7633, .T. ) ;
#4399 = FACE_OUTER_BOUND ( 'NONE', #6735, .T. ) ;
#4400 = EDGE_CURVE ( 'NONE', #3765, #8325, #2362, .T. ) ;
#4401 = DIRECTION ( 'NONE',  ( 1.000000000000000000, 0.000000000000000000, 0.000000000000000000 ) ) ;
#4402 = CARTESIAN_POINT ( 'NONE',  ( 0.000000000000000000, 7.653668647300657213, -18.47759065022568237 ) ) ;
#4403 = CIRCLE ( 'NONE', #1486, 2.999999999999999556 ) ;
#4404 = VERTEX_POINT ( 'NONE', #1993 ) ;
#4405 = VERTEX_POINT ( 'NONE', #595 ) ;
#4406 = AXIS2_PLACEMENT_3D ( 'NONE', #6445, #4939, #7146 ) ;
#4407 = DIRECTION ( 'NONE',  ( 0.000000000000000000, 0.000000000000000000, -1.000000000000000000 ) ) ;
#4408 = CARTESIAN_POINT ( 'NONE',  ( 15.70011763207405231, 9.048619709455117288, 47.70011763207404698 ) ) ;
#4409 = VECTOR ( 'NONE', #7739, 1000.000000000000000 ) ;
#4410 = AXIS2_PLACEMENT_3D ( 'NONE', #2786, #5720, #8634 ) ;
#4411 = DIRECTION ( 'NONE',  ( -0.000000000000000000, -0.000000000000000000, 1.000000000000000000 ) ) ;
#4412 = AXIS2_PLACEMENT_3D ( 'NONE', #3848, #6063, #6013 ) ;
#4413 = ADVANCED_FACE ( 'NONE', ( #1260 ), #5787, .F. ) ;
#4414 = EDGE_CURVE ( 'NONE', #4692, #4881, #7125, .T. ) ;
#4415 = CONICAL_SURFACE ( 'NONE', #8559, 17.50000000000000000, 0.7853981633974552734 ) ;
#4416 = PLANE ( 'NONE',  #6360 ) ;
#4417 = EDGE_CURVE ( 'NONE', #3211, #7343, #473, .T. ) ;
#4418 = EDGE_CURVE ( 'NONE', #6367, #1975, #1979, .T. ) ;
#4419 = UNCERTAINTY_MEASURE_WITH_UNIT (LENGTH_MEASURE( 1.000000000000000082E-05 ), #1594, 'distance_accuracy_value', 'NONE');
#4420 = CARTESIAN_POINT ( 'NONE',  ( 9.364477336218625325, 62.15368297487813010, 0.9332626224471926024 ) ) ;
#4421 = ORIENTED_EDGE ( 'NONE', *, *, #1125, .T. ) ;
#4422 = VERTEX_POINT ( 'NONE', #5016 ) ;
#4423 = ORIENTED_EDGE ( 'NONE', *, *, #6737, .F. ) ;
#4424 = DIRECTION ( 'NONE',  ( 0.9994148367277967404, -0.0008129226918946904062, -0.03419536935095459501 ) ) ;
#4425 = ORIENTED_EDGE ( 'NONE', *, *, #8629, .F. ) ;
#4426 = DIRECTION ( 'NONE',  ( 0.000000000000000000, 0.000000000000000000, 1.000000000000000000 ) ) ;
#4427 = VECTOR ( 'NONE', #5114, 1000.000000000000000 ) ;
#4428 = CARTESIAN_POINT ( 'NONE',  ( 0.000000000000000000, 0.000000000000000000, 63.00000000000002842 ) ) ;
#4429 = FACE_OUTER_BOUND ( 'NONE', #4090, .T. ) ;
#4430 = LINE ( 'NONE', #2366, #6024 ) ;
#4431 = DIRECTION ( 'NONE',  ( -1.000000000000000000, 0.000000000000000000, -0.000000000000000000 ) ) ;
#4432 = CARTESIAN_POINT ( 'NONE',  ( 6.000000000000000888, 7.347880794884120722E-16, 1.000000000000000000 ) ) ;
#4433 = AXIS2_PLACEMENT_3D ( 'NONE', #2680, #605, #6428 ) ;
#4434 = EDGE_CURVE ( 'NONE', #5694, #7596, #7219, .T. ) ;
#4435 = ORIENTED_EDGE ( 'NONE', *, *, #5536, .F. ) ;
#4436 = VECTOR ( 'NONE', #5154, 1000.000000000000000 ) ;
#4437 = DIRECTION ( 'NONE',  ( -1.000000000000000000, 0.000000000000000000, 0.000000000000000000 ) ) ;
#4438 = ORIENTED_EDGE ( 'NONE', *, *, #7615, .T. ) ;
#4439 = EDGE_CURVE ( 'NONE', #7709, #1163, #2174, .T. ) ;
#4440 = CARTESIAN_POINT ( 'NONE',  ( 4.000000000000000000, 18.47759065022580316, -7.653668647301631545 ) ) ;
#4441 = CARTESIAN_POINT ( 'NONE',  ( 0.000000000000000000, -35.00000000000000000, 49.50000000000000000 ) ) ;
#4442 = ADVANCED_FACE ( 'NONE', ( #5880 ), #1503, .T. ) ;
#4443 = DIRECTION ( 'NONE',  ( -0.000000000000000000, -0.000000000000000000, 1.000000000000000000 ) ) ;
#4444 = CARTESIAN_POINT ( 'NONE',  ( 4.000000000000000000, 2.724839128102860991E-15, -22.00000000000000355 ) ) ;
#4445 = ORIENTED_EDGE ( 'NONE', *, *, #8643, .T. ) ;
#4446 = ORIENTED_EDGE ( 'NONE', *, *, #4439, .T. ) ;
#4447 = CARTESIAN_POINT ( 'NONE',  ( 2.813989238837719675, 27.81487630015519841, 0.9541967664096193680 ) ) ;
#4448 = ORIENTED_EDGE ( 'NONE', *, *, #3830, .T. ) ;
#4449 = DIRECTION ( 'NONE',  ( 0.7071067811865479058, 0.000000000000000000, 0.7071067811865471286 ) ) ;
#4450 = DIRECTION ( 'NONE',  ( -0.000000000000000000, -0.000000000000000000, -1.000000000000000000 ) ) ;
#4451 = CARTESIAN_POINT ( 'NONE',  ( 12.50000000000000000, 1.530808498934191127E-15, 28.50000000000000355 ) ) ;
#4452 = CARTESIAN_POINT ( 'NONE',  ( -51.96152422706631313, 30.00000000000000711, -12.99999999999999289 ) ) ;
#4453 = CARTESIAN_POINT ( 'NONE',  ( 3.499999999999999556, 0.000000000000000000, 0.000000000000000000 ) ) ;
#4454 = DIRECTION ( 'NONE',  ( -1.000000000000000000, 0.000000000000000000, 0.000000000000000000 ) ) ;
#4455 = DIRECTION ( 'NONE',  ( -0.7071067811865507924, -0.7071067811865441310, 0.000000000000000000 ) ) ;
#4456 = EDGE_CURVE ( 'NONE', #4348, #6332, #3666, .T. ) ;
#4457 = ORIENTED_EDGE ( 'NONE', *, *, #6649, .F. ) ;
#4458 = VERTEX_POINT ( 'NONE', #5834 ) ;
#4459 = CARTESIAN_POINT ( 'NONE',  ( 50.79490495164537833, -30.00000000000000000, -100.0000000000000000 ) ) ;
#4460 = ORIENTED_EDGE ( 'NONE', *, *, #4131, .T. ) ;
#4461 = EDGE_CURVE ( 'NONE', #1938, #7674, #8575, .T. ) ;
#4462 = CARTESIAN_POINT ( 'NONE',  ( -0.6837532375831764098, 28.73276100836656610, 1.738917791092793319 ) ) ;
#4463 = AXIS2_PLACEMENT_3D ( 'NONE', #3917, #6991, #4784 ) ;
#4464 = CARTESIAN_POINT ( 'NONE',  ( -22.50000000000000000, -7.855833012397050680E-14, 15.00000000000000000 ) ) ;
#4465 = CARTESIAN_POINT ( 'NONE',  ( -26.21170834203224231, 53.97171801779369105, -2.612255525622730001 ) ) ;
#4466 = VERTEX_POINT ( 'NONE', #5206 ) ;
#4467 = ORIENTED_EDGE ( 'NONE', *, *, #4294, .T. ) ;
#4468 = DIRECTION ( 'NONE',  ( 1.000000000000000000, -0.000000000000000000, -0.000000000000000000 ) ) ;
#4469 = CARTESIAN_POINT ( 'NONE',  ( 0.000000000000000000, 0.000000000000000000, 2.999999999999999112 ) ) ;
#4470 = CYLINDRICAL_SURFACE ( 'NONE', #7965, 6.000000000000001776 ) ;
#4471 = PRODUCT ( '1-Center Box', '1-Center Box', '', ( #5236 ) ) ;
#4472 = FACE_OUTER_BOUND ( 'NONE', #2841, .T. ) ;
#4473 = DIRECTION ( 'NONE',  ( 0.000000000000000000, 0.000000000000000000, 1.000000000000000000 ) ) ;
#4474 = DIRECTION ( 'NONE',  ( -1.000000000000000000, 0.000000000000000000, -0.000000000000000000 ) ) ;
#4475 = EDGE_CURVE ( 'NONE', #7912, #6850, #7508, .T. ) ;
#4476 = VERTEX_POINT ( 'NONE', #4386 ) ;
#4477 = DIRECTION ( 'NONE',  ( -1.000000000000000000, -0.000000000000000000, -0.000000000000000000 ) ) ;
#4478 = VERTEX_POINT ( 'NONE', #6227 ) ;
#4479 = VECTOR ( 'NONE', #4764, 1000.000000000000000 ) ;
#4480 = FACE_OUTER_BOUND ( 'NONE', #2224, .T. ) ;
#4481 = DIRECTION ( 'NONE',  ( -1.000000000000000000, 0.000000000000000000, 0.000000000000000000 ) ) ;
#4482 = DIRECTION ( 'NONE',  ( 1.000000000000000000, 0.000000000000000000, 0.000000000000000000 ) ) ;
#4483 = FACE_OUTER_BOUND ( 'NONE', #2794, .T. ) ;
#4484 = ORIENTED_EDGE ( 'NONE', *, *, #709, .T. ) ;
#4485 = ORIENTED_EDGE ( 'NONE', *, *, #4551, .F. ) ;
#4486 = ORIENTED_EDGE ( 'NONE', *, *, #6999, .F. ) ;
#4487 = DIRECTION ( 'NONE',  ( 1.000000000000000000, 0.000000000000000000, 0.000000000000000000 ) ) ;
#4488 = AXIS2_PLACEMENT_3D ( 'NONE', #2938, #5923, #1598 ) ;
#4489 = ORIENTED_EDGE ( 'NONE', *, *, #1007, .F. ) ;
#4490 = DIRECTION ( 'NONE',  ( 0.000000000000000000, 0.000000000000000000, -1.000000000000000000 ) ) ;
#4491 = CARTESIAN_POINT ( 'NONE',  ( -37.00000000000000711, -15.90990257669733943, -54.09009742330271564 ) ) ;
#4492 = CARTESIAN_POINT ( 'NONE',  ( -11.96410161513786008, 0.000000000000000000, 50.00000000000000000 ) ) ;
#4493 = CARTESIAN_POINT ( 'NONE',  ( 59.00000000000000000, 7.225416114969383207E-15, 25.00000000000000000 ) ) ;
#4494 = CARTESIAN_POINT ( 'NONE',  ( -0.7500000000000000000, -2.749999999999995559, 1.500000000000000000 ) ) ;
#4495 = AXIS2_PLACEMENT_3D ( 'NONE', #5488, #8273, #8418 ) ;
#4496 = DIRECTION ( 'NONE',  ( 0.000000000000000000, 0.000000000000000000, -1.000000000000000000 ) ) ;
#4497 = CYLINDRICAL_SURFACE ( 'NONE', #1037, 0.7500000000013684609 ) ;
#4498 = VERTEX_POINT ( 'NONE', #5926 ) ;
#4499 = VERTEX_POINT ( 'NONE', #6608 ) ;
#4500 = CIRCLE ( 'NONE', #1583, 6.000000000000000888 ) ;
#4501 = DIRECTION ( 'NONE',  ( -1.000000000000000000, 0.000000000000000000, 0.000000000000000000 ) ) ;
#4502 = CARTESIAN_POINT ( 'NONE',  ( 60.00000000000000000, -12.50000000000000000, -100.0000000000000000 ) ) ;
#4503 = ORIENTED_EDGE ( 'NONE', *, *, #269, .T. ) ;
#4504 = CARTESIAN_POINT ( 'NONE',  ( 7.180166011355011868, 26.02777777777776791, 0.000000000000000000 ) ) ;
#4505 = EDGE_CURVE ( 'NONE', #8041, #2851, #27, .T. ) ;
#4506 = FACE_BOUND ( 'NONE', #1092, .T. ) ;
#4507 = CARTESIAN_POINT ( 'NONE',  ( 15.00000000000000000, 1.836970198721029589E-15, 10.00000000000000000 ) ) ;
#4508 = EDGE_LOOP ( 'NONE', ( #2520, #1014, #7003, #2619 ) ) ;
#4509 = ADVANCED_FACE ( 'NONE', ( #8759 ), #4284, .T. ) ;
#4510 = EDGE_LOOP ( 'NONE', ( #5631, #591 ) ) ;
#4511 = CARTESIAN_POINT ( 'NONE',  ( 23.57597564296054671, 17.54340043416276629, 60.90601756443965087 ) ) ;
#4512 = AXIS2_PLACEMENT_3D ( 'NONE', #1324, #5574, #1966 ) ;
#4513 = LINE ( 'NONE', #5344, #1162 ) ;
#4514 = LINE ( 'NONE', #7441, #2426 ) ;
#4515 = CIRCLE ( 'NONE', #6364, 15.00000000000000000 ) ;
#4516 = CARTESIAN_POINT ( 'NONE',  ( 0.000000000000000000, 0.000000000000000000, 64.00000000000000000 ) ) ;
#4517 = DIRECTION ( 'NONE',  ( -0.000000000000000000, 0.000000000000000000, 1.000000000000000000 ) ) ;
#4518 = EDGE_CURVE ( 'NONE', #9037, #8187, #69, .T. ) ;
#4519 = CARTESIAN_POINT ( 'NONE',  ( -37.00000000000000000, -13.96446609406728712, -95.00000000000000000 ) ) ;
#4520 = DIRECTION ( 'NONE',  ( 0.000000000000000000, 0.000000000000000000, 1.000000000000000000 ) ) ;
#4521 = CARTESIAN_POINT ( 'NONE',  ( -15.99999999999999645, -43.00000000000000000, -7.366666666666667140 ) ) ;
#4522 = VERTEX_POINT ( 'NONE', #1552 ) ;
#4523 = DIRECTION ( 'NONE',  ( -1.000000000000000000, -0.000000000000000000, -0.000000000000000000 ) ) ;
#4524 = VECTOR ( 'NONE', #6785, 999.9999999999998863 ) ;
#4525 = ORIENTED_EDGE ( 'NONE', *, *, #1009, .T. ) ;
#4526 = DIRECTION ( 'NONE',  ( 0.000000000000000000, 0.000000000000000000, -1.000000000000000000 ) ) ;
#4527 = DIRECTION ( 'NONE',  ( -1.000000000000000000, 0.000000000000000000, -0.000000000000000000 ) ) ;
#4528 = VECTOR ( 'NONE', #8296, 1000.000000000000000 ) ;
#4529 = CARTESIAN_POINT ( 'NONE',  ( 4.000000000000000000, 14.14213562373247868, 14.14213562373282329 ) ) ;
#4530 = ADVANCED_FACE ( 'NONE', ( #7409 ), #2942, .F. ) ;
#4531 = CARTESIAN_POINT ( 'NONE',  ( -12.37436867076458036, 12.37436867076458036, 44.37436867076458213 ) ) ;
#4532 = ADVANCED_FACE ( 'NONE', ( #3717 ), #7363, .T. ) ;
#4533 = VERTEX_POINT ( 'NONE', #8851 ) ;
#4534 = EDGE_CURVE ( 'NONE', #8189, #2635, #2276, .T. ) ;
#4535 = EDGE_CURVE ( 'NONE', #1699, #6770, #822, .T. ) ;
#4536 = VERTEX_POINT ( 'NONE', #6695 ) ;
#4537 =( GEOMETRIC_REPRESENTATION_CONTEXT ( 3 ) GLOBAL_UNCERTAINTY_ASSIGNED_CONTEXT ( ( #1627 ) ) GLOBAL_UNIT_ASSIGNED_CONTEXT ( ( #4150, #7077, #1212 ) ) REPRESENTATION_CONTEXT ( 'NONE', 'WORKASPACE' ) );
#4538 = ORIENTED_EDGE ( 'NONE', *, *, #6688, .T. ) ;
#4539 = DIRECTION ( 'NONE',  ( 1.000000000000000000, 0.000000000000000000, 0.000000000000000000 ) ) ;
#4540 = VERTEX_POINT ( 'NONE', #116 ) ;
#4541 = CARTESIAN_POINT ( 'NONE',  ( -0.7500000000000000000, -2.749999999999995559, 1.500000000000000000 ) ) ;
#4542 = CARTESIAN_POINT ( 'NONE',  ( 4.119968255444916849E-15, 3.500000000000000000, 1.500000000000000000 ) ) ;
#4543 = CARTESIAN_POINT ( 'NONE',  ( 4.000000000000000000, 20.00000000000120437, -1.559999999998198161 ) ) ;
#4544 = DIRECTION ( 'NONE',  ( 0.000000000000000000, -1.000000000000000000, 0.000000000000000000 ) ) ;
#4545 = AXIS2_PLACEMENT_3D ( 'NONE', #5866, #5091, #767 ) ;
#4546 = VECTOR ( 'NONE', #9018, 1000.000000000000000 ) ;
#4547 = FACE_BOUND ( 'NONE', #3556, .T. ) ;
#4548 = EDGE_CURVE ( 'NONE', #794, #3854, #5980, .T. ) ;
#4549 = DIRECTION ( 'NONE',  ( 8.659560562354963673E-17, -0.7071067811865451302, 0.7071067811865500152 ) ) ;
#4550 = CARTESIAN_POINT ( 'NONE',  ( 4.000000000000000000, 7.653668647300657213, -19.22759065022689384 ) ) ;
#4551 = EDGE_CURVE ( 'NONE', #5692, #8610, #9030, .T. ) ;
#4552 = ORIENTED_EDGE ( 'NONE', *, *, #7107, .F. ) ;
#4553 = EDGE_LOOP ( 'NONE', ( #9025, #3094, #4129, #8159 ) ) ;
#4554 = EDGE_CURVE ( 'NONE', #2584, #4960, #8184, .T. ) ;
#4555 = AXIS2_PLACEMENT_3D ( 'NONE', #7419, #1463, #788 ) ;
#4556 = DIRECTION ( 'NONE',  ( 0.000000000000000000, 0.000000000000000000, 1.000000000000000000 ) ) ;
#4557 = CARTESIAN_POINT ( 'NONE',  ( -30.00000000000000000, 0.000000000000000000, 3.000000000000052847 ) ) ;
#4558 = ORIENTED_EDGE ( 'NONE', *, *, #6547, .F. ) ;
#4559 = CARTESIAN_POINT ( 'NONE',  ( -5.103771271004210242, 27.45068023253072909, 0.9147230066269097515 ) ) ;
#4560 = AXIS2_PLACEMENT_3D ( 'NONE', #7700, #304, #971 ) ;
#4561 = DIRECTION ( 'NONE',  ( 0.000000000000000000, 0.000000000000000000, 1.000000000000000000 ) ) ;
#4562 = CARTESIAN_POINT ( 'NONE',  ( 2.341162148116626263, -28.48643429264087246, 1.580564902411995210 ) ) ;
#4563 = AXIS2_PLACEMENT_3D ( 'NONE', #1642, #5248, #8174 ) ;
#4564 = EDGE_LOOP ( 'NONE', ( #2974, #6838 ) ) ;
#4565 = VERTEX_POINT ( 'NONE', #5306 ) ;
#4566 = APPLICATION_PROTOCOL_DEFINITION ( 'draft international standard', 'automotive_design', 1998, #4133 ) ;
#4567 = AXIS2_PLACEMENT_3D ( 'NONE', #4364, #3736, #4501 ) ;
#4568 = AXIS2_PLACEMENT_3D ( 'NONE', #337, #5391, #1006 ) ;
#4569 = CARTESIAN_POINT ( 'NONE',  ( 27.00000000000000000, 43.00000000000000000, 11.99999999999999645 ) ) ;
#4570 = CARTESIAN_POINT ( 'NONE',  ( -37.22467645238203460, -47.05659850664382304, -5.608807313787673721 ) ) ;
#4571 = CARTESIAN_POINT ( 'NONE',  ( 4.000000000000000000, 14.14213562373112154, -15.70213562373078098 ) ) ;
#4572 = AXIS2_PLACEMENT_3D ( 'NONE', #2007, #7190, #6248 ) ;
#4573 = LINE ( 'NONE', #3033, #8475 ) ;
#4574 = CARTESIAN_POINT ( 'NONE',  ( 37.00000000000000000, -30.00000000000000000, -78.96446609406730488 ) ) ;
#4575 = CARTESIAN_POINT ( 'NONE',  ( 0.000000000000000000, 0.000000000000000000, 64.00000000000000000 ) ) ;
#4576 = CARTESIAN_POINT ( 'NONE',  ( 4.078200081724819626, -26.91636876093598119, 0.2219739674467010593 ) ) ;
#4577 =( BOUNDED_CURVE ( )  B_SPLINE_CURVE ( 3, ( #8972, #1089, #1818, #9159 ),
 .UNSPECIFIED., .F., .T. ) 
 B_SPLINE_CURVE_WITH_KNOTS ( ( 4, 4 ),
 ( 3.233473586661880450, 3.279793965437969749 ),
 .UNSPECIFIED. ) 
 CURVE ( )  GEOMETRIC_REPRESENTATION_ITEM ( )  RATIONAL_B_SPLINE_CURVE ( ( 1.000000000000000000, 0.9998212098678860293, 0.9998212098678860293, 1.000000000000000000 ) ) 
 REPRESENTATION_ITEM ( '' )  );
#4578 = ORIENTED_EDGE ( 'NONE', *, *, #3830, .F. ) ;
#4579 = CARTESIAN_POINT ( 'NONE',  ( -18.49999999999997513, 2.265596578422600241E-15, 64.00000000000000000 ) ) ;
#4580 = AXIS2_PLACEMENT_3D ( 'NONE', #7624, #6241, #2637 ) ;
#4581 = ORIENTED_EDGE ( 'NONE', *, *, #1288, .T. ) ;
#4582 = FACE_OUTER_BOUND ( 'NONE', #1001, .T. ) ;
#4583 = FACE_OUTER_BOUND ( 'NONE', #6851, .T. ) ;
#4584 = CARTESIAN_POINT ( 'NONE',  ( 5.000000000000000000, -7.653668647303860872, -19.22759065022669134 ) ) ;
#4585 = DIRECTION ( 'NONE',  ( 0.000000000000000000, 0.000000000000000000, -1.000000000000000000 ) ) ;
#4586 = CIRCLE ( 'NONE', #439, 0.7500000000017874591 ) ;
#4587 = VECTOR ( 'NONE', #2757, 999.9999999999998863 ) ;
#4588 = ORIENTED_EDGE ( 'NONE', *, *, #7882, .F. ) ;
#4589 = EDGE_LOOP ( 'NONE', ( #6282, #5691, #3330 ) ) ;
#4590 = ORIENTED_EDGE ( 'NONE', *, *, #2624, .T. ) ;
#4591 = EDGE_LOOP ( 'NONE', ( #4969, #8488, #6750, #4191 ) ) ;
#4592 = CARTESIAN_POINT ( 'NONE',  ( 0.000000000000000000, 18.47759065022580316, -8.403668647301632433 ) ) ;
#4593 = CARTESIAN_POINT ( 'NONE',  ( -39.50000000000000711, 29.99999999999999645, -82.50000000000000000 ) ) ;
#4594 = VECTOR ( 'NONE', #5871, 1000.000000000000000 ) ;
#4595 = DIRECTION ( 'NONE',  ( -1.000000000000000000, 0.000000000000000000, 0.000000000000000000 ) ) ;
#4596 = EDGE_CURVE ( 'NONE', #5974, #3120, #973, .T. ) ;
#4597 = EDGE_CURVE ( 'NONE', #9178, #3545, #1787, .T. ) ;
#4598 = DIRECTION ( 'NONE',  ( -1.000000000000000000, -0.000000000000000000, -0.000000000000000000 ) ) ;
#4599 = DIRECTION ( 'NONE',  ( 0.000000000000000000, -1.000000000000000000, 0.000000000000000000 ) ) ;
#4600 = LINE ( 'NONE', #1209, #8855 ) ;
#4601 = CARTESIAN_POINT ( 'NONE',  ( 0.000000000000000000, -22.50000000000000355, 5.000000000000000000 ) ) ;
#4602 = ORIENTED_EDGE ( 'NONE', *, *, #6377, .F. ) ;
#4603 = EDGE_LOOP ( 'NONE', ( #4369, #1748 ) ) ;
#4604 = CARTESIAN_POINT ( 'NONE',  ( 27.00000000000000355, 35.00000000000000000, 59.00000000000000000 ) ) ;
#4605 = ORIENTED_EDGE ( 'NONE', *, *, #3953, .F. ) ;
#4606 = CARTESIAN_POINT ( 'NONE',  ( 0.000000000000000000, 0.000000000000000000, 0.000000000000000000 ) ) ;
#4607 = CARTESIAN_POINT ( 'NONE',  ( 0.000000000000000000, -22.50000000000000355, 2.000000000000013767 ) ) ;
#4608 = ORIENTED_EDGE ( 'NONE', *, *, #5261, .T. ) ;
#4609 = CARTESIAN_POINT ( 'NONE',  ( -37.00000000000000000, -30.00000000000000000, -12.99999999999999822 ) ) ;
#4610 = FACE_OUTER_BOUND ( 'NONE', #5138, .T. ) ;
#4611 = CARTESIAN_POINT ( 'NONE',  ( -6.000000000000000888, 0.000000000000000000, 5.000000000000000000 ) ) ;
#4612 = ORIENTED_EDGE ( 'NONE', *, *, #3731, .T. ) ;
#4613 = ORIENTED_EDGE ( 'NONE', *, *, #1236, .T. ) ;
#4614 = CYLINDRICAL_SURFACE ( 'NONE', #5001, 6.000000000000000888 ) ;
#4615 = CIRCLE ( 'NONE', #773, 6.000000000000000888 ) ;
#4616 = CARTESIAN_POINT ( 'NONE',  ( 50.79490495164537833, -30.00000000000000355, -82.50000000000001421 ) ) ;
#4617 = APPLICATION_CONTEXT ( 'automotive_design' ) ;
#4618 = CARTESIAN_POINT ( 'NONE',  ( -31.99999999999999289, -34.99999999999999289, 5.000000000000004441 ) ) ;
#4619 =( NAMED_UNIT ( * ) SI_UNIT ( $, .STERADIAN. ) SOLID_ANGLE_UNIT ( ) );
#4620 = FACE_OUTER_BOUND ( 'NONE', #8645, .T. ) ;
#4621 = CARTESIAN_POINT ( 'NONE',  ( -26.99999999999996092, -29.99999999999996447, 0.000000000000000000 ) ) ;
#4622 = AXIS2_PLACEMENT_3D ( 'NONE', #7081, #544, #4343 ) ;
#4623 = VERTEX_POINT ( 'NONE', #7656 ) ;
#4624 = CARTESIAN_POINT ( 'NONE',  ( 5.000000000000000000, -7.653668647303860872, -18.47759065022490432 ) ) ;
#4625 = VERTEX_POINT ( 'NONE', #5449 ) ;
#4626 = ADVANCED_BREP_SHAPE_REPRESENTATION ( '', ( #190, #1614 ), #7287 ) ;
#4627 = DIRECTION ( 'NONE',  ( -1.000000000000000000, 0.000000000000000000, 0.000000000000000000 ) ) ;
#4628 = DIRECTION ( 'NONE',  ( -0.000000000000000000, -0.000000000000000000, -1.000000000000000000 ) ) ;
#4629 = DIRECTION ( 'NONE',  ( -0.000000000000000000, -0.000000000000000000, -1.000000000000000000 ) ) ;
#4630 = ADVANCED_FACE ( 'NONE', ( #8991, #7749 ), #1069, .F. ) ;
#4631 =( BOUNDED_CURVE ( )  B_SPLINE_CURVE ( 3, ( #8185, #8142, #1601, #4531 ),
 .UNSPECIFIED., .F., .T. ) 
 B_SPLINE_CURVE_WITH_KNOTS ( ( 4, 4 ),
 ( 0.000000000000000000, 0.7853981633974485010 ),
 .UNSPECIFIED. ) 
 CURVE ( )  GEOMETRIC_REPRESENTATION_ITEM ( )  RATIONAL_B_SPLINE_CURVE ( ( 1.000000000000000000, 0.9492530216741911220, 0.9492530216741911220, 1.000000000000000000 ) ) 
 REPRESENTATION_ITEM ( '' )  );
#4632 = DIRECTION ( 'NONE',  ( -1.000000000000000000, 0.000000000000000000, 0.000000000000000000 ) ) ;
#4633 = ORIENTED_EDGE ( 'NONE', *, *, #1957, .F. ) ;
#4634 = AXIS2_PLACEMENT_3D ( 'NONE', #1349, #9269, #5689 ) ;
#4635 = ORIENTED_EDGE ( 'NONE', *, *, #6758, .T. ) ;
#4636 = EDGE_CURVE ( 'NONE', #5576, #956, #7659, .T. ) ;
#4637 = ORIENTED_EDGE ( 'NONE', *, *, #3586, .F. ) ;
#4638 = ORIENTED_EDGE ( 'NONE', *, *, #2647, .F. ) ;
#4639 = DIRECTION ( 'NONE',  ( 0.000000000000000000, 0.000000000000000000, 1.000000000000000000 ) ) ;
#4640 = DIRECTION ( 'NONE',  ( -0.7071067811865463515, 8.659560562354919300E-17, 0.7071067811865487940 ) ) ;
#4641 = DIRECTION ( 'NONE',  ( -0.000000000000000000, -0.000000000000000000, 1.000000000000000000 ) ) ;
#4642 = DIRECTION ( 'NONE',  ( 1.000000000000000000, 0.000000000000000000, 0.000000000000000000 ) ) ;
#4643 = CARTESIAN_POINT ( 'NONE',  ( 0.000000000000000000, 0.000000000000000000, 27.50000000000000355 ) ) ;
#4644 = FACE_OUTER_BOUND ( 'NONE', #6876, .T. ) ;
#4645 = AXIS2_PLACEMENT_3D ( 'NONE', #4440, #7263, #7311 ) ;
#4646 = FACE_OUTER_BOUND ( 'NONE', #6301, .T. ) ;
#4647 = VERTEX_POINT ( 'NONE', #2517 ) ;
#4648 = ORIENTED_EDGE ( 'NONE', *, *, #7399, .F. ) ;
#4649 = CARTESIAN_POINT ( 'NONE',  ( -17.50000000000000355, 2.143131898507868643E-15, 1.000000000000021760 ) ) ;
#4650 = ORIENTED_EDGE ( 'NONE', *, *, #711, .F. ) ;
#4651 = CARTESIAN_POINT ( 'NONE',  ( 15.00000000000000000, 1.836970198721029589E-15, 27.50000000000000355 ) ) ;
#4652 = ORIENTED_EDGE ( 'NONE', *, *, #894, .T. ) ;
#4653 = AXIS2_PLACEMENT_3D ( 'NONE', #6368, #7170, #1357 ) ;
#4654 = PRODUCT_RELATED_PRODUCT_CATEGORY ( 'part', '', ( #9448 ) ) ;
#4655 = DIRECTION ( 'NONE',  ( 0.000000000000000000, 0.7071067811865473507, 0.7071067811865477948 ) ) ;
#4656 = ADVANCED_FACE ( 'NONE', ( #4052 ), #9183, .F. ) ;
#4657 = ADVANCED_FACE ( 'NONE', ( #3278 ), #6984, .F. ) ;
#4658 = ADVANCED_FACE ( 'NONE', ( #8373 ), #215, .T. ) ;
#4659 = FACE_BOUND ( 'NONE', #3923, .T. ) ;
#4660 = DIRECTION ( 'NONE',  ( 0.6785983445458481089, -0.2810846377148337183, 0.6785983445458404484 ) ) ;
#4661 = EDGE_LOOP ( 'NONE', ( #8476, #5123 ) ) ;
#4662 = ORIENTED_EDGE ( 'NONE', *, *, #2469, .F. ) ;
#4663 = EDGE_CURVE ( 'NONE', #1694, #2461, #5981, .T. ) ;
#4664 = CIRCLE ( 'NONE', #5583, 18.49999999999998934 ) ;
#4665 = DIRECTION ( 'NONE',  ( 0.000000000000000000, 0.000000000000000000, -1.000000000000000000 ) ) ;
#4666 = FACE_OUTER_BOUND ( 'NONE', #7437, .T. ) ;
#4667 = CARTESIAN_POINT ( 'NONE',  ( 53.29490495164537833, 18.67545040036925386, -90.28901569369799063 ) ) ;
#4668 = SURFACE_STYLE_FILL_AREA ( #340 ) ;
#4669 = LINE ( 'NONE', #9172, #3822 ) ;
#4670 = ADVANCED_FACE ( 'NONE', ( #6936 ), #6079, .T. ) ;
#4671 = DIRECTION ( 'NONE',  ( -0.000000000000000000, 1.000000000000000000, -0.000000000000000000 ) ) ;
#4672 = EDGE_LOOP ( 'NONE', ( #668, #4117, #8487, #4578 ) ) ;
#4673 = AXIS2_PLACEMENT_3D ( 'NONE', #3117, #5523, #6055 ) ;
#4674 =( NAMED_UNIT ( * ) SI_UNIT ( $, .STERADIAN. ) SOLID_ANGLE_UNIT ( ) );
#4675 = ORIENTED_EDGE ( 'NONE', *, *, #758, .T. ) ;
#4676 = EDGE_CURVE ( 'NONE', #6525, #6171, #3048, .T. ) ;
#4677 = LINE ( 'NONE', #1695, #650 ) ;
#4678 = CIRCLE ( 'NONE', #2833, 6.000000000000000888 ) ;
#4679 = LINE ( 'NONE', #2566, #6401 ) ;
#4680 = CARTESIAN_POINT ( 'NONE',  ( 0.7500000000000000000, 0.7500000000000000000, 1.500000000000000000 ) ) ;
#4681 = AXIS2_PLACEMENT_3D ( 'NONE', #2192, #7423, #5940 ) ;
#4682 = CARTESIAN_POINT ( 'NONE',  ( -39.50000000000000711, 29.99999999999999645, -82.50000000000000000 ) ) ;
#4683 = EDGE_LOOP ( 'NONE', ( #3306, #2435, #481, #1210 ) ) ;
#4684 = ORIENTED_EDGE ( 'NONE', *, *, #9101, .F. ) ;
#4685 = EDGE_LOOP ( 'NONE', ( #5224, #764, #4633, #6780, #5599, #3465, #5861, #4959, #2178, #1521, #5813, #5262, #7767, #4130, #6330, #7744 ) ) ;
#4686 = ORIENTED_EDGE ( 'NONE', *, *, #5824, .F. ) ;
#4687 = DIRECTION ( 'NONE',  ( 1.000000000000000000, 0.000000000000000000, 0.000000000000000000 ) ) ;
#4688 = DIRECTION ( 'NONE',  ( 0.000000000000000000, -0.7071067811865473507, -0.7071067811865477948 ) ) ;
#4689 = DIRECTION ( 'NONE',  ( -0.000000000000000000, -0.000000000000000000, -1.000000000000000000 ) ) ;
#4690 = DIRECTION ( 'NONE',  ( 0.000000000000000000, 0.000000000000000000, 1.000000000000000000 ) ) ;
#4691 = CARTESIAN_POINT ( 'NONE',  ( 28.50000000000000355, 2.364097880450372804E-13, 1.500000000000041078 ) ) ;
#4692 = VERTEX_POINT ( 'NONE', #8806 ) ;
#4693 = DIRECTION ( 'NONE',  ( 0.000000000000000000, 0.000000000000000000, -1.000000000000000000 ) ) ;
#4694 = ORIENTED_EDGE ( 'NONE', *, *, #1731, .F. ) ;
#4695 = VERTEX_POINT ( 'NONE', #4728 ) ;
#4696 = ADVANCED_FACE ( 'NONE', ( #5358 ), #1885, .F. ) ;
#4697 = CARTESIAN_POINT ( 'NONE',  ( 0.000000000000000000, 0.000000000000000000, 4.000000000000000000 ) ) ;
#4698 = ORIENTED_EDGE ( 'NONE', *, *, #7654, .T. ) ;
#4699 = FACE_OUTER_BOUND ( 'NONE', #3987, .T. ) ;
#4700 = DIRECTION ( 'NONE',  ( 0.000000000000000000, 0.000000000000000000, 1.000000000000000000 ) ) ;
#4701 = ORIENTED_EDGE ( 'NONE', *, *, #9139, .T. ) ;
#4702 = CIRCLE ( 'NONE', #5625, 13.66147716702868031 ) ;
#4703 = CYLINDRICAL_SURFACE ( 'NONE', #3796, 7.250000000000002665 ) ;
#4704 = DIRECTION ( 'NONE',  ( -1.000000000000000000, 0.000000000000000000, 0.000000000000000000 ) ) ;
#4705 = PLANE ( 'NONE',  #884 ) ;
#4706 = AXIS2_PLACEMENT_3D ( 'NONE', #3334, #3286, #2577 ) ;
#4707 = ORIENTED_EDGE ( 'NONE', *, *, #4461, .T. ) ;
#4708 = EDGE_LOOP ( 'NONE', ( #2971, #394 ) ) ;
#4709 = CONTEXT_DEPENDENT_SHAPE_REPRESENTATION ( #2289, #9372 ) ;
#4710 = ADVANCED_FACE ( 'NONE', ( #7601 ), #6127, .F. ) ;
#4711 = PLANE ( 'NONE',  #4412 ) ;
#4712 = CIRCLE ( 'NONE', #5173, 1.560000000000000719 ) ;
#4713 = ADVANCED_FACE ( 'NONE', ( #8321 ), #1742, .F. ) ;
#4714 = EDGE_CURVE ( 'NONE', #1397, #8147, #305, .T. ) ;
#4715 = EDGE_CURVE ( 'NONE', #8690, #3384, #2844, .T. ) ;
#4716 = LINE ( 'NONE', #4667, #4524 ) ;
#4717 = DIRECTION ( 'NONE',  ( 0.000000000000000000, 0.000000000000000000, -1.000000000000000000 ) ) ;
#4718 = CARTESIAN_POINT ( 'NONE',  ( 60.00000000000000000, -3.673940397442057600E-15, -70.00000000000000000 ) ) ;
#4719 = AXIS2_PLACEMENT_3D ( 'NONE', #3692, #4368, #5046 ) ;
#4720 = CARTESIAN_POINT ( 'NONE',  ( 53.29490495164537833, -27.56180520566615044, -41.61356529332876875 ) ) ;
#4721 = VECTOR ( 'NONE', #7144, 1000.000000000000000 ) ;
#4722 = ORIENTED_EDGE ( 'NONE', *, *, #3123, .T. ) ;
#4723 = CARTESIAN_POINT ( 'NONE',  ( 60.00000000000000000, -1.836970198721028011E-15, -85.00000000000000000 ) ) ;
#4724 = ORIENTED_EDGE ( 'NONE', *, *, #8544, .F. ) ;
#4725 = CARTESIAN_POINT ( 'NONE',  ( 0.000000000000000000, 30.00000000000000000, 0.000000000000000000 ) ) ;
#4726 = FACE_OUTER_BOUND ( 'NONE', #7608, .T. ) ;
#4727 = AXIS2_PLACEMENT_3D ( 'NONE', #6575, #3684, #7235 ) ;
#4728 = CARTESIAN_POINT ( 'NONE',  ( 0.000000000000000000, 18.47759065022658120, 8.403668647301545391 ) ) ;
#4729 = CIRCLE ( 'NONE', #1151, 60.00000000000000000 ) ;
#4730 = DIRECTION ( 'NONE',  ( -1.000000000000000000, -0.000000000000000000, -0.000000000000000000 ) ) ;
#4731 = ADVANCED_FACE ( 'NONE', ( #531 ), #7885, .T. ) ;
#4732 = EDGE_LOOP ( 'NONE', ( #1770, #74, #6159, #1074 ) ) ;
#4733 = VECTOR ( 'NONE', #8675, 1000.000000000000000 ) ;
#4734 = EDGE_LOOP ( 'NONE', ( #3295, #7708, #4590, #2483 ) ) ;
#4735 = VERTEX_POINT ( 'NONE', #8701 ) ;
#4736 = ORIENTED_EDGE ( 'NONE', *, *, #3843, .T. ) ;
#4737 = CYLINDRICAL_SURFACE ( 'NONE', #3882, 17.50000000000000355 ) ;
#4738 = ADVANCED_FACE ( 'NONE', ( #9321 ), #7072, .F. ) ;
#4739 = CARTESIAN_POINT ( 'NONE',  ( -0.7500000000000000000, 2.750000000000002665, 0.000000000000000000 ) ) ;
#4740 = AXIS2_PLACEMENT_3D ( 'NONE', #7275, #8906, #176 ) ;
#4741 = CARTESIAN_POINT ( 'NONE',  ( 12.37436867076458036, -12.37436867076458036, 44.37436867076458213 ) ) ;
#4742 = CARTESIAN_POINT ( 'NONE',  ( -48.15955140082795793, 36.58521010404107443, -10.14640895491552897 ) ) ;
#4743 = CARTESIAN_POINT ( 'NONE',  ( -12.50000000000000000, 0.000000000000000000, 50.00000000000000000 ) ) ;
#4744 = ORIENTED_EDGE ( 'NONE', *, *, #6826, .T. ) ;
#4745 = VERTEX_POINT ( 'NONE', #1983 ) ;
#4746 = DIRECTION ( 'NONE',  ( -0.4999999999999977240, 0.000000000000000000, 0.8660254037844399289 ) ) ;
#4747 = AXIS2_PLACEMENT_3D ( 'NONE', #2438, #7562, #9000 ) ;
#4748 = ORIENTED_EDGE ( 'NONE', *, *, #7365, .T. ) ;
#4749 = FACE_BOUND ( 'NONE', #5079, .T. ) ;
#4750 = AXIS2_PLACEMENT_3D ( 'NONE', #8800, #2903, #738 ) ;
#4751 = ORIENTED_EDGE ( 'NONE', *, *, #709, .F. ) ;
#4752 =( REPRESENTATION_RELATIONSHIP ('NONE','NONE', #1933, #8501 ) REPRESENTATION_RELATIONSHIP_WITH_TRANSFORMATION ( #8635 )SHAPE_REPRESENTATION_RELATIONSHIP( ) );
#4753 = CARTESIAN_POINT ( 'NONE',  ( 0.000000000000000000, 0.000000000000000000, 50.00000000000000000 ) ) ;
#4754 = EDGE_CURVE ( 'NONE', #8277, #3453, #1070, .T. ) ;
#4755 = FACE_BOUND ( 'NONE', #9446, .T. ) ;
#4756 = CARTESIAN_POINT ( 'NONE',  ( -12.37436867076458036, -12.37436867076458036, 44.37436867076458213 ) ) ;
#4757 = ORIENTED_EDGE ( 'NONE', *, *, #8346, .T. ) ;
#4758 = ORIENTED_EDGE ( 'NONE', *, *, #1831, .T. ) ;
#4759 = ADVANCED_FACE ( 'NONE', ( #4860 ), #9224, .F. ) ;
#4760 = ITEM_DEFINED_TRANSFORMATION ( 'NONE', 'NONE', #6083,  #1614 ) ;
#4761 = CONICAL_SURFACE ( 'NONE', #6287, 2.499999999999998668, 0.7853981633974461696 ) ;
#4762 = DIRECTION ( 'NONE',  ( -1.000000000000000000, 0.000000000000000000, 0.000000000000000000 ) ) ;
#4763 = LINE ( 'NONE', #7642, #9120 ) ;
#4764 = DIRECTION ( 'NONE',  ( -0.000000000000000000, -0.000000000000000000, -1.000000000000000000 ) ) ;
#4765 = DIRECTION ( 'NONE',  ( -0.000000000000000000, 1.000000000000000000, -0.000000000000000000 ) ) ;
#4766 = CARTESIAN_POINT ( 'NONE',  ( -0.7500000000000000000, -0.7500000000000000000, 1.500000000000000000 ) ) ;
#4767 = ORIENTED_EDGE ( 'NONE', *, *, #3931, .F. ) ;
#4768 = DIRECTION ( 'NONE',  ( -0.000000000000000000, -0.000000000000000000, -1.000000000000000000 ) ) ;
#4769 = VECTOR ( 'NONE', #5572, 1000.000000000000000 ) ;
#4770 = ORIENTED_EDGE ( 'NONE', *, *, #1850, .T. ) ;
#4771 = DIRECTION ( 'NONE',  ( 0.7071067811865493491, 0.000000000000000000, -0.7071067811865456854 ) ) ;
#4772 = DIRECTION ( 'NONE',  ( 0.7071067811865494601, 0.000000000000000000, -0.7071067811865455743 ) ) ;
#4773 = CARTESIAN_POINT ( 'NONE',  ( 60.00000000000000000, 15.90990257669733943, -54.09009742330271564 ) ) ;
#4774 = EDGE_CURVE ( 'NONE', #6226, #7541, #5511, .T. ) ;
#4775 = CARTESIAN_POINT ( 'NONE',  ( -15.00000000000000000, 0.000000000000000000, 20.00000000000000000 ) ) ;
#4776 = CIRCLE ( 'NONE', #177, 3.000000000000000000 ) ;
#4777 = EDGE_CURVE ( 'NONE', #5110, #4995, #7652, .T. ) ;
#4778 = ORIENTED_EDGE ( 'NONE', *, *, #6947, .F. ) ;
#4779 = ORIENTED_EDGE ( 'NONE', *, *, #3115, .T. ) ;
#4780 = DIRECTION ( 'NONE',  ( -1.000000000000000000, 0.000000000000000000, 0.000000000000000000 ) ) ;
#4781 = VERTEX_POINT ( 'NONE', #3416 ) ;
#4782 = CYLINDRICAL_SURFACE ( 'NONE', #1110, 7.250000000000002665 ) ;
#4783 = CARTESIAN_POINT ( 'NONE',  ( 0.000000000000000000, -7.653668647303860872, -19.22759065022669134 ) ) ;
#4784 = DIRECTION ( 'NONE',  ( 0.000000000000000000, 0.000000000000000000, -1.000000000000000000 ) ) ;
#4785 = CARTESIAN_POINT ( 'NONE',  ( 6.000000000000000888, -22.50000000000000355, 2.000000000000013767 ) ) ;
#4786 = DIRECTION ( 'NONE',  ( 0.000000000000000000, 0.7071067811865456854, 0.7071067811865493491 ) ) ;
#4787 = EDGE_LOOP ( 'NONE', ( #4457, #8965, #5052, #3405 ) ) ;
#4788 = ORIENTED_EDGE ( 'NONE', *, *, #6421, .F. ) ;
#4789 = PLANE ( 'NONE',  #2845 ) ;
#4790 = VERTEX_POINT ( 'NONE', #6316 ) ;
#4791 = DIRECTION ( 'NONE',  ( 0.000000000000000000, 0.000000000000000000, -1.000000000000000000 ) ) ;
#4792 = VERTEX_POINT ( 'NONE', #5590 ) ;
#4793 = CIRCLE ( 'NONE', #1873, 1.560000000000134168 ) ;
#4794 = CARTESIAN_POINT ( 'NONE',  ( 0.000000000000000000, 0.000000000000000000, 28.50000000000000355 ) ) ;
#4795 = VECTOR ( 'NONE', #8034, 1000.000000000000000 ) ;
#4796 = CARTESIAN_POINT ( 'NONE',  ( 53.29490495164537833, -15.90990257669733943, -51.09009742330271564 ) ) ;
#4797 = CARTESIAN_POINT ( 'NONE',  ( -37.22467645238198486, 47.05659850664388699, -5.608807313787648852 ) ) ;
#4798 = ORIENTED_EDGE ( 'NONE', *, *, #2303, .T. ) ;
#4799 = VERTEX_POINT ( 'NONE', #4229 ) ;
#4800 = CIRCLE ( 'NONE', #656, 1.000000000000000888 ) ;
#4801 = DIRECTION ( 'NONE',  ( -1.000000000000000000, 0.000000000000000000, 0.000000000000000000 ) ) ;
#4802 = CARTESIAN_POINT ( 'NONE',  ( 0.000000000000000000, 0.000000000000000000, 2.999999999999999112 ) ) ;
#4803 = EDGE_CURVE ( 'NONE', #3965, #6009, #9268, .T. ) ;
#4804 = DIRECTION ( 'NONE',  ( -0.000000000000000000, -0.000000000000000000, 1.000000000000000000 ) ) ;
#4805 = VECTOR ( 'NONE', #3551, 1000.000000000000000 ) ;
#4806 = CYLINDRICAL_SURFACE ( 'NONE', #4495, 7.250000000000002665 ) ;
#4807 = ORIENTED_EDGE ( 'NONE', *, *, #7230, .F. ) ;
#4808 = VERTEX_POINT ( 'NONE', #5734 ) ;
#4809 = DIRECTION ( 'NONE',  ( 1.000000000000000000, 0.000000000000000000, 0.000000000000000000 ) ) ;
#4810 = CARTESIAN_POINT ( 'NONE',  ( -27.00000000000000000, -43.00000000000000000, 11.99999999999999645 ) ) ;
#4811 = CIRCLE ( 'NONE', #6051, 2.999999999999999112 ) ;
#4812 = EDGE_CURVE ( 'NONE', #2492, #3951, #7931, .T. ) ;
#4813 = DIRECTION ( 'NONE',  ( -1.000000000000000000, 0.000000000000000000, 0.000000000000000000 ) ) ;
#4814 = LINE ( 'NONE', #5591, #5244 ) ;
#4815 = AXIS2_PLACEMENT_3D ( 'NONE', #666, #2879, #1577 ) ;
#4816 = DIRECTION ( 'NONE',  ( 0.000000000000000000, 0.000000000000000000, 1.000000000000000000 ) ) ;
#4817 = ORIENTED_EDGE ( 'NONE', *, *, #5890, .F. ) ;
#4818 = EDGE_LOOP ( 'NONE', ( #625, #3815 ) ) ;
#4819 = DIRECTION ( 'NONE',  ( 0.000000000000000000, 0.000000000000000000, 1.000000000000000000 ) ) ;
#4820 = ORIENTED_EDGE ( 'NONE', *, *, #7995, .F. ) ;
#4821 = FACE_BOUND ( 'NONE', #604, .T. ) ;
#4822 = DIRECTION ( 'NONE',  ( 1.000000000000000000, 0.000000000000000000, 0.000000000000000000 ) ) ;
#4823 = EDGE_CURVE ( 'NONE', #7976, #4945, #3814, .T. ) ;
#4824 = COLOUR_RGB ( '',0.7921568627450980005, 0.8196078431372548767, 0.9333333333333333481 ) ;
#4825 = LINE ( 'NONE', #6325, #7218 ) ;
#4826 = EDGE_CURVE ( 'NONE', #975, #2905, #1375, .T. ) ;
#4827 = AXIS2_PLACEMENT_3D ( 'NONE', #2176, #4246, #7176 ) ;
#4828 = FACE_OUTER_BOUND ( 'NONE', #8862, .T. ) ;
#4829 = EDGE_CURVE ( 'NONE', #5974, #4623, #2301, .T. ) ;
#4830 = EDGE_CURVE ( 'NONE', #7998, #7322, #8603, .T. ) ;
#4831 = DIRECTION ( 'NONE',  ( 1.000000000000000000, 0.000000000000000000, 0.000000000000000000 ) ) ;
#4832 = ORIENTED_EDGE ( 'NONE', *, *, #1717, .T. ) ;
#4833 = VERTEX_POINT ( 'NONE', #631 ) ;
#4834 = PLANE ( 'NONE',  #5305 ) ;
#4835 = ORIENTED_EDGE ( 'NONE', *, *, #7543, .T. ) ;
#4836 = DIRECTION ( 'NONE',  ( -0.000000000000000000, -0.000000000000000000, 1.000000000000000000 ) ) ;
#4837 = CARTESIAN_POINT ( 'NONE',  ( -31.99999999999999289, 0.000000000000000000, 32.00000000000000000 ) ) ;
#4838 = VERTEX_POINT ( 'NONE', #1249 ) ;
#4839 = PLANE ( 'NONE',  #2554 ) ;
#4840 = DIRECTION ( 'NONE',  ( -1.000000000000000000, 0.000000000000000000, 0.000000000000000000 ) ) ;
#4841 = CIRCLE ( 'NONE', #5008, 0.7500000000001906253 ) ;
#4842 = EDGE_CURVE ( 'NONE', #5859, #438, #8424, .T. ) ;
#4843 = ADVANCED_FACE ( 'NONE', ( #2027 ), #4952, .F. ) ;
#4844 = DIRECTION ( 'NONE',  ( -0.000000000000000000, -0.000000000000000000, -1.000000000000000000 ) ) ;
#4845 = CARTESIAN_POINT ( 'NONE',  ( 26.02777777777776791, 7.180166011355005651, 0.000000000000000000 ) ) ;
#4846 = ADVANCED_FACE ( 'NONE', ( #6500 ), #4761, .T. ) ;
#4847 = EDGE_LOOP ( 'NONE', ( #2065, #6986, #9354, #3419 ) ) ;
#4848 = ORIENTED_EDGE ( 'NONE', *, *, #4294, .F. ) ;
#4849 = AXIS2_PLACEMENT_3D ( 'NONE', #398, #4819, #451 ) ;
#4850 = DIRECTION ( 'NONE',  ( 0.000000000000000000, 0.000000000000000000, 1.000000000000000000 ) ) ;
#4851 = DIRECTION ( 'NONE',  ( 0.000000000000000000, -0.000000000000000000, 1.000000000000000000 ) ) ;
#4852 = AXIS2_PLACEMENT_3D ( 'NONE', #1582, #155, #7491 ) ;
#4853 = CARTESIAN_POINT ( 'NONE',  ( 37.22467645238197775, -47.05659850664388699, -0.5000000000000038858 ) ) ;
#4854 = DIRECTION ( 'NONE',  ( 0.000000000000000000, -0.000000000000000000, -1.000000000000000000 ) ) ;
#4855 = EDGE_LOOP ( 'NONE', ( #9434, #7832, #5773, #7104 ) ) ;
#4856 = ORIENTED_EDGE ( 'NONE', *, *, #6550, .T. ) ;
#4857 = EDGE_LOOP ( 'NONE', ( #8209, #1605, #1423, #4767 ) ) ;
#4858 = CARTESIAN_POINT ( 'NONE',  ( -2.999999999999842792, -22.50000000000000355, 15.00000000000000000 ) ) ;
#4859 = CARTESIAN_POINT ( 'NONE',  ( -37.00000000000000000, -30.00000000000000000, -13.00000000000001066 ) ) ;
#4860 = FACE_OUTER_BOUND ( 'NONE', #2179, .T. ) ;
#4861 = CARTESIAN_POINT ( 'NONE',  ( -20.14434505884618076, 53.53579249963519970, -2.801156583491412722 ) ) ;
#4862 = EDGE_CURVE ( 'NONE', #233, #31, #7203, .T. ) ;
#4863 = AXIS2_PLACEMENT_3D ( 'NONE', #2940, #3716, #6648 ) ;
#4864 = ORIENTED_EDGE ( 'NONE', *, *, #4994, .F. ) ;
#4865 = ORIENTED_EDGE ( 'NONE', *, *, #5637, .F. ) ;
#4866 = VERTEX_POINT ( 'NONE', #2316 ) ;
#4867 = AXIS2_PLACEMENT_3D ( 'NONE', #7339, #1432, #761 ) ;
#4868 = DIRECTION ( 'NONE',  ( -1.000000000000000000, -0.000000000000000000, -0.000000000000000000 ) ) ;
#4869 = CIRCLE ( 'NONE', #9468, 3.000000000000002665 ) ;
#4870 = CARTESIAN_POINT ( 'NONE',  ( -5.000000000000000888, 6.735557395310443009E-16, 0.000000000000000000 ) ) ;
#4871 = VECTOR ( 'NONE', #2209, 1000.000000000000000 ) ;
#4872 = CYLINDRICAL_SURFACE ( 'NONE', #4622, 15.00000000000000000 ) ;
#4873 = AXIS2_PLACEMENT_3D ( 'NONE', #7873, #620, #8781 ) ;
#4874 = CIRCLE ( 'NONE', #6123, 6.000000000000000888 ) ;
#4875 = DIRECTION ( 'NONE',  ( -1.000000000000000000, 0.000000000000000000, 0.000000000000000000 ) ) ;
#4876 = CYLINDRICAL_SURFACE ( 'NONE', #59, 1.560000000002236709 ) ;
#4877 = ORIENTED_EDGE ( 'NONE', *, *, #6002, .F. ) ;
#4878 = ORIENTED_EDGE ( 'NONE', *, *, #805, .T. ) ;
#4879 =( BOUNDED_CURVE ( )  B_SPLINE_CURVE ( 3, ( #9035, #4043, #6886, #436 ),
 .UNSPECIFIED., .F., .F. ) 
 B_SPLINE_CURVE_WITH_KNOTS ( ( 4, 4 ),
 ( 5.497787143782137953, 7.068583470577034511 ),
 .UNSPECIFIED. ) 
 CURVE ( )  GEOMETRIC_REPRESENTATION_ITEM ( )  RATIONAL_B_SPLINE_CURVE ( ( 1.000000000000000000, 0.8047378541243649375, 0.8047378541243649375, 1.000000000000000000 ) ) 
 REPRESENTATION_ITEM ( '' )  );
#4880 = FACE_OUTER_BOUND ( 'NONE', #3422, .T. ) ;
#4881 = VERTEX_POINT ( 'NONE', #9465 ) ;
#4882 = EDGE_CURVE ( 'NONE', #2987, #8436, #8838, .T. ) ;
#4883 = CARTESIAN_POINT ( 'NONE',  ( 16.00000000000000000, -49.08300322764474544, -4.730698601353946486 ) ) ;
#4884 = LINE ( 'NONE', #4260, #7484 ) ;
#4885 = AXIS2_PLACEMENT_3D ( 'NONE', #5854, #9474, #5999 ) ;
#4886 = EDGE_CURVE ( 'NONE', #5944, #5804, #2598, .T. ) ;
#4887 = DIRECTION ( 'NONE',  ( 0.000000000000000000, 0.000000000000000000, 1.000000000000000000 ) ) ;
#4888 = FACE_OUTER_BOUND ( 'NONE', #5223, .T. ) ;
#4889 = CYLINDRICAL_SURFACE ( 'NONE', #4973, 3.000000000000002665 ) ;
#4890 = AXIS2_PLACEMENT_3D ( 'NONE', #1608, #3866, #4687 ) ;
#4891 = CARTESIAN_POINT ( 'NONE',  ( -6.702350214711367826, -26.42345776824586423, 0.2543657081580636414 ) ) ;
#4892 = EDGE_CURVE ( 'NONE', #8532, #3965, #6764, .T. ) ;
#4893 = ORIENTED_EDGE ( 'NONE', *, *, #1532, .F. ) ;
#4894 = AXIS2_PLACEMENT_3D ( 'NONE', #4296, #2673, #8665 ) ;
#4895 = ORIENTED_EDGE ( 'NONE', *, *, #7439, .T. ) ;
#4896 = CONTEXT_DEPENDENT_SHAPE_REPRESENTATION ( #5732, #3546 ) ;
#4897 = AXIS2_PLACEMENT_3D ( 'NONE', #8462, #6787, #1062 ) ;
#4898 = PLANE ( 'NONE',  #3443 ) ;
#4899 = DIRECTION ( 'NONE',  ( 0.000000000000000000, 0.7071067811865473507, 0.7071067811865477948 ) ) ;
#4900 = DIRECTION ( 'NONE',  ( 1.000000000000000000, 0.000000000000000000, 0.000000000000000000 ) ) ;
#4901 = ORIENTED_EDGE ( 'NONE', *, *, #8035, .F. ) ;
#4902 = ORIENTED_EDGE ( 'NONE', *, *, #3599, .F. ) ;
#4903 = VERTEX_POINT ( 'NONE', #5868 ) ;
#4904 = ORIENTED_EDGE ( 'NONE', *, *, #145, .F. ) ;
#4905 = CARTESIAN_POINT ( 'NONE',  ( 59.00000000000000000, 7.286648454926750781E-15, 25.00000000000000000 ) ) ;
#4906 = FACE_OUTER_BOUND ( 'NONE', #64, .T. ) ;
#4907 = DIRECTION ( 'NONE',  ( -1.000000000000000000, 0.000000000000000000, 0.000000000000000000 ) ) ;
#4908 = DIRECTION ( 'NONE',  ( -1.000000000000000000, -0.000000000000000000, -0.000000000000000000 ) ) ;
#4909 = DIRECTION ( 'NONE',  ( -1.000000000000000000, -0.000000000000000000, -0.000000000000000000 ) ) ;
#4910 = VERTEX_POINT ( 'NONE', #811 ) ;
#4911 = CARTESIAN_POINT ( 'NONE',  ( 72.75414293302374347, 30.00000000000000000, -51.44494782735612404 ) ) ;
#4912 = DIRECTION ( 'NONE',  ( 0.000000000000000000, -0.5535840618632023036, -0.8327933035579949683 ) ) ;
#4913 = VERTEX_POINT ( 'NONE', #6639 ) ;
#4914 = DIRECTION ( 'NONE',  ( -0.000000000000000000, -0.000000000000000000, 1.000000000000000000 ) ) ;
#4915 = CARTESIAN_POINT ( 'NONE',  ( 0.000000000000000000, -34.00000000000001421, 49.50000000000000000 ) ) ;
#4916 = ADVANCED_FACE ( 'NONE', ( #5820 ), #8791, .F. ) ;
#4917 = AXIS2_PLACEMENT_3D ( 'NONE', #3060, #4544, #81 ) ;
#4918 = DIRECTION ( 'NONE',  ( 0.7071067811865456854, 0.7071067811865493491, 3.960316634274392569E-15 ) ) ;
#4919 = CARTESIAN_POINT ( 'NONE',  ( 37.00000000000000000, 15.90990257669733943, -57.09009742330271564 ) ) ;
#4920 = ADVANCED_FACE ( 'NONE', ( #5195 ), #4470, .F. ) ;
#4921 = FACE_OUTER_BOUND ( 'NONE', #408, .T. ) ;
#4922 = PRODUCT_DEFINITION_SHAPE ( 'NONE', 'NONE',  #3945 ) ;
#4923 = ORIENTED_EDGE ( 'NONE', *, *, #4051, .F. ) ;
#4924 = EDGE_LOOP ( 'NONE', ( #5011, #4240, #8567, #3665 ) ) ;
#4925 = CARTESIAN_POINT ( 'NONE',  ( -2.819222834329253136, 27.81181297095831084, 0.9517275379012117842 ) ) ;
#4926 = ORIENTED_EDGE ( 'NONE', *, *, #1240, .T. ) ;
#4927 = LINE ( 'NONE', #5706, #295 ) ;
#4928 = DIRECTION ( 'NONE',  ( -1.000000000000000000, 0.000000000000000000, 0.000000000000000000 ) ) ;
#4929 = DIRECTION ( 'NONE',  ( 1.000000000000000000, 0.000000000000000000, 0.000000000000000000 ) ) ;
#4930 = CARTESIAN_POINT ( 'NONE',  ( 32.00000000000000711, -29.99999999999996447, 64.00000000000000000 ) ) ;
#4931 = CARTESIAN_POINT ( 'NONE',  ( 0.000000000000000000, 0.000000000000000000, 20.49999999999999645 ) ) ;
#4932 = CARTESIAN_POINT ( 'NONE',  ( -31.99999999999999289, 2.143131898507868643E-15, 49.50000000000000000 ) ) ;
#4933 = ORIENTED_EDGE ( 'NONE', *, *, #3335, .T. ) ;
#4934 = ORIENTED_EDGE ( 'NONE', *, *, #3446, .F. ) ;
#4935 = AXIS2_PLACEMENT_3D ( 'NONE', #6696, #5982, #781 ) ;
#4936 = DIRECTION ( 'NONE',  ( 0.000000000000000000, -0.7071067811865473507, -0.7071067811865477948 ) ) ;
#4937 = EDGE_CURVE ( 'NONE', #5417, #550, #2615, .T. ) ;
#4938 = EDGE_CURVE ( 'NONE', #5908, #386, #3497, .T. ) ;
#4939 = DIRECTION ( 'NONE',  ( 0.000000000000000000, 0.000000000000000000, 1.000000000000000000 ) ) ;
#4940 = EDGE_CURVE ( 'NONE', #1266, #5535, #7494, .T. ) ;
#4941 = DIRECTION ( 'NONE',  ( -0.000000000000000000, -0.000000000000000000, -1.000000000000000000 ) ) ;
#4942 = DIRECTION ( 'NONE',  ( -0.000000000000000000, -0.000000000000000000, -1.000000000000000000 ) ) ;
#4943 = EDGE_CURVE ( 'NONE', #6332, #4348, #143, .T. ) ;
#4944 = DIRECTION ( 'NONE',  ( 0.000000000000000000, 0.000000000000000000, -1.000000000000000000 ) ) ;
#4945 = VERTEX_POINT ( 'NONE', #8747 ) ;
#4946 = ORIENTED_EDGE ( 'NONE', *, *, #4518, .T. ) ;
#4947 = AXIS2_PLACEMENT_3D ( 'NONE', #9317, #6314, #5587 ) ;
#4948 = ORIENTED_EDGE ( 'NONE', *, *, #5760, .F. ) ;
#4949 = ORIENTED_EDGE ( 'NONE', *, *, #8121, .F. ) ;
#4950 = LINE ( 'NONE', #2024, #7242 ) ;
#4951 = DIRECTION ( 'NONE',  ( -1.000000000000000000, 0.000000000000000000, 0.000000000000000000 ) ) ;
#4952 = CYLINDRICAL_SURFACE ( 'NONE', #5361, 3.000000000000002665 ) ;
#4953 = EDGE_CURVE ( 'NONE', #3755, #3545, #5913, .T. ) ;
#4954 = CIRCLE ( 'NONE', #972, 2.999999999999999112 ) ;
#4955 = CARTESIAN_POINT ( 'NONE',  ( 2.749999999999996447, -0.7500000000000000000, 1.500000000000000000 ) ) ;
#4956 = EDGE_CURVE ( 'NONE', #4498, #2916, #1822, .T. ) ;
#4957 = CYLINDRICAL_SURFACE ( 'NONE', #8245, 17.50000000000000000 ) ;
#4958 = EDGE_CURVE ( 'NONE', #6408, #3516, #4295, .T. ) ;
#4959 = ORIENTED_EDGE ( 'NONE', *, *, #2604, .F. ) ;
#4960 = VERTEX_POINT ( 'NONE', #1540 ) ;
#4961 = ORIENTED_EDGE ( 'NONE', *, *, #1735, .F. ) ;
#4962 = FACE_BOUND ( 'NONE', #4014, .T. ) ;
#4963 = AXIS2_PLACEMENT_3D ( 'NONE', #5376, #319, #3203 ) ;
#4964 = CARTESIAN_POINT ( 'NONE',  ( -15.70011763207405586, -9.048619709455111959, 16.29988236792594591 ) ) ;
#4965 = CARTESIAN_POINT ( 'NONE',  ( -15.99999999999999645, 43.00000000000000000, 11.99999999999999645 ) ) ;
#4966 = DIRECTION ( 'NONE',  ( 0.000000000000000000, 0.000000000000000000, -1.000000000000000000 ) ) ;
#4967 = DIRECTION ( 'NONE',  ( -0.000000000000000000, -0.000000000000000000, -1.000000000000000000 ) ) ;
#4968 = ORIENTED_EDGE ( 'NONE', *, *, #7942, .T. ) ;
#4969 = ORIENTED_EDGE ( 'NONE', *, *, #1525, .T. ) ;
#4970 = CARTESIAN_POINT ( 'NONE',  ( -0.8594978869055871495, 28.44192451354557605, 1.454119780865612999 ) ) ;
#4971 = EDGE_LOOP ( 'NONE', ( #482, #9252, #7037, #5645 ) ) ;
#4972 = CARTESIAN_POINT ( 'NONE',  ( -7.180166011355011868, 26.02777777777776436, 0.000000000000000000 ) ) ;
#4973 = AXIS2_PLACEMENT_3D ( 'NONE', #512, #9249, #7188 ) ;
#4974 = FACE_OUTER_BOUND ( 'NONE', #8338, .T. ) ;
#4975 = DIRECTION ( 'NONE',  ( 0.000000000000000000, 0.000000000000000000, -1.000000000000000000 ) ) ;
#4976 = AXIS2_PLACEMENT_3D ( 'NONE', #571, #3363, #6306 ) ;
#4977 = CARTESIAN_POINT ( 'NONE',  ( 0.000000000000000000, 0.000000000000000000, 20.00000000000000000 ) ) ;
#4978 = CARTESIAN_POINT ( 'NONE',  ( 0.000000000000000000, 17.50000000000000000, 49.50000000000000000 ) ) ;
#4979 = DIRECTION ( 'NONE',  ( 0.7071067811865444641, -0.7071067811865505703, -0.000000000000000000 ) ) ;
#4980 = ORIENTED_EDGE ( 'NONE', *, *, #4006, .T. ) ;
#4981 = VECTOR ( 'NONE', #3031, 1000.000000000000000 ) ;
#4982 = ORIENTED_EDGE ( 'NONE', *, *, #3603, .F. ) ;
#4983 = FACE_BOUND ( 'NONE', #989, .T. ) ;
#4984 = ITEM_DEFINED_TRANSFORMATION ( 'NONE', 'NONE', #6993,  #1614 ) ;
#4985 = ORIENTED_EDGE ( 'NONE', *, *, #2850, .F. ) ;
#4986 = CARTESIAN_POINT ( 'NONE',  ( -53.29490495164537833, -30.00000000000000000, -100.0000000000000000 ) ) ;
#4987 =( BOUNDED_CURVE ( )  B_SPLINE_CURVE ( 3, ( #1876, #7101, #1198, #5627 ),
 .UNSPECIFIED., .F., .T. ) 
 B_SPLINE_CURVE_WITH_KNOTS ( ( 4, 4 ),
 ( 3.233473586661879118, 3.279793965437967973 ),
 .UNSPECIFIED. ) 
 CURVE ( )  GEOMETRIC_REPRESENTATION_ITEM ( )  RATIONAL_B_SPLINE_CURVE ( ( 1.000000000000000000, 0.9998212098678860293, 0.9998212098678860293, 1.000000000000000000 ) ) 
 REPRESENTATION_ITEM ( '' )  );
#4988 = CARTESIAN_POINT ( 'NONE',  ( -50.79490495164537833, 29.99999999999999645, -82.50000000000000000 ) ) ;
#4989 = DIRECTION ( 'NONE',  ( -0.000000000000000000, -0.000000000000000000, -1.000000000000000000 ) ) ;
#4990 = MANIFOLD_SOLID_BREP ( 'Pah5', #3635 ) ;
#4991 = ORIENTED_EDGE ( 'NONE', *, *, #9233, .T. ) ;
#4992 = ORIENTED_EDGE ( 'NONE', *, *, #3239, .T. ) ;
#4993 = ORIENTED_EDGE ( 'NONE', *, *, #3426, .T. ) ;
#4994 = EDGE_CURVE ( 'NONE', #7343, #6251, #5809, .T. ) ;
#4995 = VERTEX_POINT ( 'NONE', #1490 ) ;
#4996 = ADVANCED_FACE ( 'NONE', ( #4429 ), #838, .F. ) ;
#4997 = CARTESIAN_POINT ( 'NONE',  ( 28.50000000000000711, -0.4241759143233731488, 1.500000000000038192 ) ) ;
#4998 = EDGE_CURVE ( 'NONE', #1940, #3913, #769, .T. ) ;
#4999 = ADVANCED_FACE ( 'NONE', ( #9171 ), #5904, .T. ) ;
#5000 = DIRECTION ( 'NONE',  ( -1.000000000000000000, 0.000000000000000000, 0.000000000000000000 ) ) ;
#5001 = AXIS2_PLACEMENT_3D ( 'NONE', #3078, #8931, #3124 ) ;
#5002 = DIRECTION ( 'NONE',  ( -1.000000000000000000, 0.000000000000000000, 0.000000000000000000 ) ) ;
#5003 = PRODUCT_DEFINITION_SHAPE ( 'NONE', 'NONE',  #9482 ) ;
#5004 = DIRECTION ( 'NONE',  ( 0.000000000000000000, 0.000000000000000000, 1.000000000000000000 ) ) ;
#5005 = DIRECTION ( 'NONE',  ( 1.000000000000000000, -0.000000000000000000, 0.000000000000000000 ) ) ;
#5006 = ORIENTED_EDGE ( 'NONE', *, *, #5463, .T. ) ;
#5007 = VECTOR ( 'NONE', #2287, 1000.000000000000000 ) ;
#5008 = AXIS2_PLACEMENT_3D ( 'NONE', #6997, #460, #2725 ) ;
#5009 = DIRECTION ( 'NONE',  ( -1.000000000000000000, 0.000000000000000000, 0.000000000000000000 ) ) ;
#5010 = EDGE_CURVE ( 'NONE', #9366, #1900, #2218, .T. ) ;
#5011 = ORIENTED_EDGE ( 'NONE', *, *, #5238, .F. ) ;
#5012 = DIRECTION ( 'NONE',  ( 0.000000000000000000, 0.000000000000000000, 1.000000000000000000 ) ) ;
#5013 = CARTESIAN_POINT ( 'NONE',  ( 0.000000000000000000, 0.000000000000000000, 0.000000000000000000 ) ) ;
#5014 = VECTOR ( 'NONE', #5009, 1000.000000000000000 ) ;
#5015 = EDGE_CURVE ( 'NONE', #55, #4223, #6834, .T. ) ;
#5016 = CARTESIAN_POINT ( 'NONE',  ( -14.49999999999998401, 0.000000000000000000, 27.50000000000000355 ) ) ;
#5017 = VECTOR ( 'NONE', #7884, 1000.000000000000000 ) ;
#5018 = LINE ( 'NONE', #644, #2937 ) ;
#5019 = AXIS2_PLACEMENT_3D ( 'NONE', #5098, #8030, #7355 ) ;
#5020 = CARTESIAN_POINT ( 'NONE',  ( 0.000000000000000000, 0.000000000000000000, 1.000000000000021760 ) ) ;
#5021 = ORIENTED_EDGE ( 'NONE', *, *, #700, .T. ) ;
#5022 = AXIS2_PLACEMENT_3D ( 'NONE', #5906, #7975, #1385 ) ;
#5023 = EDGE_CURVE ( 'NONE', #1684, #8859, #4716, .T. ) ;
#5024 = ORIENTED_EDGE ( 'NONE', *, *, #4862, .T. ) ;
#5025 = DIRECTION ( 'NONE',  ( 0.000000000000000000, 0.000000000000000000, 1.000000000000000000 ) ) ;
#5026 = AXIS2_PLACEMENT_3D ( 'NONE', #5081, #7334, #5278 ) ;
#5027 = ORIENTED_EDGE ( 'NONE', *, *, #2259, .T. ) ;
#5028 = DIRECTION ( 'NONE',  ( 1.000000000000000000, 0.000000000000000000, 0.000000000000000000 ) ) ;
#5029 = DIRECTION ( 'NONE',  ( -0.000000000000000000, -0.000000000000000000, -1.000000000000000000 ) ) ;
#5030 = CYLINDRICAL_SURFACE ( 'NONE', #3620, 7.250000000000002665 ) ;
#5031 = VECTOR ( 'NONE', #6490, 1000.000000000000000 ) ;
#5032 = CARTESIAN_POINT ( 'NONE',  ( 0.000000000000000000, -22.50000000000000355, 2.000000000000013767 ) ) ;
#5033 = CIRCLE ( 'NONE', #218, 18.50000000000001776 ) ;
#5034 = AXIS2_PLACEMENT_3D ( 'NONE', #6096, #6955, #3878 ) ;
#5035 = DIRECTION ( 'NONE',  ( -0.6785983445458477759, 0.2810846377148170649, 0.6785983445458477759 ) ) ;
#5036 = DIRECTION ( 'NONE',  ( 0.000000000000000000, 0.000000000000000000, -1.000000000000000000 ) ) ;
#5037 = EDGE_LOOP ( 'NONE', ( #1145, #1328, #8691, #1378 ) ) ;
#5038 = ORIENTED_EDGE ( 'NONE', *, *, #6777, .T. ) ;
#5039 = CIRCLE ( 'NONE', #286, 13.66147716702868031 ) ;
#5040 = DIRECTION ( 'NONE',  ( 0.000000000000000000, 0.000000000000000000, 1.000000000000000000 ) ) ;
#5041 = DIRECTION ( 'NONE',  ( -1.000000000000000000, 0.000000000000000000, 0.000000000000000000 ) ) ;
#5042 = ADVANCED_FACE ( 'NONE', ( #6066, #382 ), #2606, .T. ) ;
#5043 = VECTOR ( 'NONE', #7051, 1000.000000000000000 ) ;
#5044 = VECTOR ( 'NONE', #4287, 1000.000000000000000 ) ;
#5045 = DIRECTION ( 'NONE',  ( 0.000000000000000000, 0.000000000000000000, 1.000000000000000000 ) ) ;
#5046 = DIRECTION ( 'NONE',  ( 1.000000000000000000, 0.000000000000000000, 0.000000000000000000 ) ) ;
#5047 = ORIENTED_EDGE ( 'NONE', *, *, #4414, .T. ) ;
#5048 = ADVANCED_FACE ( 'NONE', ( #7547 ), #5347, .F. ) ;
#5049 = ORIENTED_EDGE ( 'NONE', *, *, #2739, .T. ) ;
#5050 = VERTEX_POINT ( 'NONE', #5437 ) ;
#5051 = AXIS2_PLACEMENT_3D ( 'NONE', #3896, #3175, #7692 ) ;
#5052 = ORIENTED_EDGE ( 'NONE', *, *, #6254, .T. ) ;
#5053 = LINE ( 'NONE', #2116, #3458 ) ;
#5054 = DIRECTION ( 'NONE',  ( 0.000000000000000000, 0.000000000000000000, 1.000000000000000000 ) ) ;
#5055 = CARTESIAN_POINT ( 'NONE',  ( -3.500000000000000000, 4.119968255444916849E-15, 1.500000000000000000 ) ) ;
#5056 = CARTESIAN_POINT ( 'NONE',  ( 0.000000000000000000, -7.653668647301985040, 18.47759065022880520 ) ) ;
#5057 = CARTESIAN_POINT ( 'NONE',  ( 3.000000000000000444, 3.673940397442060361E-16, 20.49999999999999645 ) ) ;
#5058 = VERTEX_POINT ( 'NONE', #1776 ) ;
#5059 = CARTESIAN_POINT ( 'NONE',  ( -31.99999999999999289, 0.000000000000000000, 32.00000000000000000 ) ) ;
#5060 = EDGE_LOOP ( 'NONE', ( #4029, #3650, #3490, #2374 ) ) ;
#5061 = FACE_BOUND ( 'NONE', #6169, .T. ) ;
#5062 = DIRECTION ( 'NONE',  ( 0.000000000000000000, 0.000000000000000000, 1.000000000000000000 ) ) ;
#5063 = ADVANCED_FACE ( 'NONE', ( #1010 ), #8312, .F. ) ;
#5065 = EDGE_CURVE ( 'NONE', #4799, #6171, #8356, .T. ) ;
#5064 = CARTESIAN_POINT ( 'NONE',  ( -38.00000000000000711, 43.00000000000000000, 11.99999999999999645 ) ) ;
#5066 = DIRECTION ( 'NONE',  ( 0.000000000000000000, 0.000000000000000000, 1.000000000000000000 ) ) ;
#5067 = ORIENTED_EDGE ( 'NONE', *, *, #3950, .F. ) ;
#5068 = VERTEX_POINT ( 'NONE', #5483 ) ;
#5069 = CARTESIAN_POINT ( 'NONE',  ( 0.000000000000000000, 22.50000000000000355, 0.000000000000000000 ) ) ;
#5070 = ORIENTED_EDGE ( 'NONE', *, *, #1426, .T. ) ;
#5071 = CARTESIAN_POINT ( 'NONE',  ( 16.50000000000000000, 2.356749903719115078E-13, 5.000000000000000000 ) ) ;
#5072 = CARTESIAN_POINT ( 'NONE',  ( 60.00000000000000000, -3.673940397442057600E-15, -70.00000000000000000 ) ) ;
#5073 = AXIS2_PLACEMENT_3D ( 'NONE', #8196, #7327, #7420 ) ;
#5074 = DIRECTION ( 'NONE',  ( 0.000000000000000000, 0.000000000000000000, -1.000000000000000000 ) ) ;
#5075 = DIRECTION ( 'NONE',  ( 0.5773502691896253980, -0.000000000000000000, 0.8164965809277263675 ) ) ;
#5076 = CYLINDRICAL_SURFACE ( 'NONE', #3141, 17.50000000000000000 ) ;
#5077 = VECTOR ( 'NONE', #9140, 1000.000000000000000 ) ;
#5078 = CARTESIAN_POINT ( 'NONE',  ( 0.000000000000000000, 7.653668647300657213, -19.22759065022689384 ) ) ;
#5079 = EDGE_LOOP ( 'NONE', ( #8145, #6578 ) ) ;
#5080 = VERTEX_POINT ( 'NONE', #8270 ) ;
#5081 = CARTESIAN_POINT ( 'NONE',  ( 0.000000000000000000, 22.50000000000000355, 5.000000000000000000 ) ) ;
#5082 = PRODUCT ( 'MAT-017', 'MAT-017', '', ( #3023 ) ) ;
#5083 = LINE ( 'NONE', #5130, #5031 ) ;
#5084 = CARTESIAN_POINT ( 'NONE',  ( 52.83333333333332860, 1.666666666666670515, -110.8333333333333570 ) ) ;
#5085 = CARTESIAN_POINT ( 'NONE',  ( 26.21170834203230982, 53.97171801779368394, -2.612255525622733554 ) ) ;
#5086 = ORIENTED_EDGE ( 'NONE', *, *, #5315, .F. ) ;
#5087 = VERTEX_POINT ( 'NONE', #4571 ) ;
#5088 = VERTEX_POINT ( 'NONE', #1099 ) ;
#5089 = CARTESIAN_POINT ( 'NONE',  ( 5.223758196597678705, 78.79028524358986374, -25.99563126639591104 ) ) ;
#5090 = VERTEX_POINT ( 'NONE', #1689 ) ;
#5091 = DIRECTION ( 'NONE',  ( 0.000000000000000000, 0.000000000000000000, -1.000000000000000000 ) ) ;
#5092 = AXIS2_PLACEMENT_3D ( 'NONE', #6743, #8079, #7445 ) ;
#5093 = DIRECTION ( 'NONE',  ( -0.000000000000000000, 0.000000000000000000, -1.000000000000000000 ) ) ;
#5094 = CARTESIAN_POINT ( 'NONE',  ( 22.50000000000000355, 0.000000000000000000, 5.000000000000000000 ) ) ;
#5095 = CARTESIAN_POINT ( 'NONE',  ( 60.00000000000000000, 15.90990257669733943, -82.90990257669729147 ) ) ;
#5096 = AXIS2_PLACEMENT_3D ( 'NONE', #8650, #2795, #6981 ) ;
#5097 = DIRECTION ( 'NONE',  ( 1.000000000000000000, 0.000000000000000000, 0.000000000000000000 ) ) ;
#5098 = CARTESIAN_POINT ( 'NONE',  ( 0.000000000000000000, 0.000000000000000000, 21.00000000000000000 ) ) ;
#5099 = ORIENTED_EDGE ( 'NONE', *, *, #7362, .T. ) ;
#5100 = CARTESIAN_POINT ( 'NONE',  ( 53.29490495164537833, 15.90990257669733943, -85.90990257669729147 ) ) ;
#5101 = EDGE_LOOP ( 'NONE', ( #8744, #4069, #7620, #8294 ) ) ;
#5102 =( REPRESENTATION_RELATIONSHIP ('NONE','NONE', #1933, #1625 ) REPRESENTATION_RELATIONSHIP_WITH_TRANSFORMATION ( #1773 )SHAPE_REPRESENTATION_RELATIONSHIP( ) );
#5103 = VECTOR ( 'NONE', #9051, 1000.000000000000000 ) ;
#5104 = EDGE_CURVE ( 'NONE', #8532, #4913, #4763, .T. ) ;
#5105 = FACE_OUTER_BOUND ( 'NONE', #9338, .T. ) ;
#5106 = DIRECTION ( 'NONE',  ( -1.000000000000000000, -0.000000000000000000, -0.000000000000000000 ) ) ;
#5107 = DIRECTION ( 'NONE',  ( -1.000000000000000000, 0.000000000000000000, 0.000000000000000000 ) ) ;
#5108 = VERTEX_POINT ( 'NONE', #916 ) ;
#5109 = CIRCLE ( 'NONE', #8496, 17.50000000000000355 ) ;
#5110 = VERTEX_POINT ( 'NONE', #5392 ) ;
#5111 = ORIENTED_EDGE ( 'NONE', *, *, #1341, .F. ) ;
#5112 = CARTESIAN_POINT ( 'NONE',  ( -57.72192878071321331, 19.00148731544555147, -33.94573509506509623 ) ) ;
#5113 = EDGE_CURVE ( 'NONE', #5930, #5629, #3298, .T. ) ;
#5114 = DIRECTION ( 'NONE',  ( -0.000000000000000000, -0.000000000000000000, 1.000000000000000000 ) ) ;
#5115 = CARTESIAN_POINT ( 'NONE',  ( 3.499999999999999556, 0.000000000000000000, 22.50000000000000000 ) ) ;
#5116 = ADVANCED_FACE ( 'NONE', ( #8415 ), #1827, .T. ) ;
#5117 = EDGE_CURVE ( 'NONE', #5750, #1024, #3267, .T. ) ;
#5118 = EDGE_CURVE ( 'NONE', #2884, #4466, #388, .T. ) ;
#5119 = CARTESIAN_POINT ( 'NONE',  ( 0.000000000000000000, 0.000000000000000000, 3.000000000000052847 ) ) ;
#5120 = DIRECTION ( 'NONE',  ( -1.000000000000000000, 0.000000000000000000, 0.000000000000000000 ) ) ;
#5121 = LINE ( 'NONE', #7376, #3439 ) ;
#5122 = FACE_OUTER_BOUND ( 'NONE', #3054, .T. ) ;
#5123 = ORIENTED_EDGE ( 'NONE', *, *, #153, .T. ) ;
#5124 = AXIS2_PLACEMENT_3D ( 'NONE', #7007, #5712, #1914 ) ;
#5125 = ORIENTED_EDGE ( 'NONE', *, *, #6511, .T. ) ;
#5126 = CARTESIAN_POINT ( 'NONE',  ( -37.00000000000000711, 15.90990257669733943, -57.09009742330271564 ) ) ;
#5127 = LINE ( 'NONE', #2966, #6117 ) ;
#5128 = VECTOR ( 'NONE', #2718, 1000.000000000000000 ) ;
#5129 = EDGE_CURVE ( 'NONE', #550, #18, #5133, .T. ) ;
#5130 = CARTESIAN_POINT ( 'NONE',  ( 37.00000000000000000, -30.00000000000000000, -95.00000000000000000 ) ) ;
#5131=STYLED_ITEM('',(#9522),#3184);
#5132 = ADVANCED_FACE ( 'NONE', ( #6164 ), #2692, .T. ) ;
#5133 = CIRCLE ( 'NONE', #5452, 11.00000000000000711 ) ;
#5134 = CARTESIAN_POINT ( 'NONE',  ( -37.00000000000000000, -30.00000000000000000, -95.00000000000000000 ) ) ;
#5135 = CARTESIAN_POINT ( 'NONE',  ( -53.29490495164537833, 15.90990257669733943, -57.09009742330271564 ) ) ;
#5136 = ORIENTED_EDGE ( 'NONE', *, *, #1293, .F. ) ;
#5137 = ORIENTED_EDGE ( 'NONE', *, *, #8055, .T. ) ;
#5138 = EDGE_LOOP ( 'NONE', ( #1790, #1231, #7102, #2335 ) ) ;
#5139 = APPLICATION_PROTOCOL_DEFINITION ( 'draft international standard', 'automotive_design', 1998, #203 ) ;
#5140 = ORIENTED_EDGE ( 'NONE', *, *, #8741, .F. ) ;
#5141 = LINE ( 'NONE', #2842, #94 ) ;
#5142 = CARTESIAN_POINT ( 'NONE',  ( 37.00000000000000000, 15.90990257669733943, -85.90990257669729147 ) ) ;
#5143 = CARTESIAN_POINT ( 'NONE',  ( 4.000000000000000000, -14.14213562373112154, 14.14213562373418220 ) ) ;
#5144 = CYLINDRICAL_SURFACE ( 'NONE', #8026, 2.999999999999999112 ) ;
#5145 = CARTESIAN_POINT ( 'NONE',  ( 5.000000000000000000, 18.47759065022658120, 7.653668647302884764 ) ) ;
#5146 = DIRECTION ( 'NONE',  ( 0.000000000000000000, 0.7071067811865473507, 0.7071067811865477948 ) ) ;
#5147 = DIRECTION ( 'NONE',  ( 0.000000000000000000, 0.000000000000000000, -1.000000000000000000 ) ) ;
#5148 = EDGE_LOOP ( 'NONE', ( #73, #588 ) ) ;
#5149 = CYLINDRICAL_SURFACE ( 'NONE', #1952, 12.50000000000000000 ) ;
#5150 = ORIENTED_EDGE ( 'NONE', *, *, #5416, .T. ) ;
#5151 = VECTOR ( 'NONE', #3580, 999.9999999999998863 ) ;
#5152 = CARTESIAN_POINT ( 'NONE',  ( -22.50000000000000355, 0.000000000000000000, 5.000000000000000000 ) ) ;
#5153 = DIRECTION ( 'NONE',  ( -0.000000000000000000, -0.000000000000000000, -1.000000000000000000 ) ) ;
#5154 = DIRECTION ( 'NONE',  ( -1.000000000000000000, -0.000000000000000000, -0.000000000000000000 ) ) ;
#5155 = EDGE_CURVE ( 'NONE', #1835, #8069, #4135, .T. ) ;
#5156 = CARTESIAN_POINT ( 'NONE',  ( 5.000000000000000000, -14.14213562373248401, -12.58213562372718641 ) ) ;
#5157 = AXIS2_PLACEMENT_3D ( 'NONE', #697, #5616, #9246 ) ;
#5158 = EDGE_LOOP ( 'NONE', ( #2182, #7260, #6816, #7319 ) ) ;
#5159 = EDGE_CURVE ( 'NONE', #5946, #8372, #2689, .T. ) ;
#5160 = ORIENTED_EDGE ( 'NONE', *, *, #4418, .T. ) ;
#5161 = CARTESIAN_POINT ( 'NONE',  ( 1.665361372754546654, 28.26799472218765530, 1.316292147329111373 ) ) ;
#5162 = ORIENTED_EDGE ( 'NONE', *, *, #1023, .F. ) ;
#5163 = CARTESIAN_POINT ( 'NONE',  ( 60.00000000000000000, 15.90990257669733943, -85.90990257669729147 ) ) ;
#5164 = CARTESIAN_POINT ( 'NONE',  ( -53.29490495164537833, -27.56180520566615044, -134.0000000000000284 ) ) ;
#5165 = CLOSED_SHELL ( 'NONE', ( #5829, #2759, #2641, #6444, #1253, #8513, #6632, #1100, #2943, #3452, #6417, #660, #4530, #4630, #7418, #6135, #6710, #5420, #3847, #6070, #3126, #4696, #6935, #5840, #4132, #4670, #6921, #7284, #78, #9109, #5063, #5132, #5116, #1931, #7820, #2495, #5592, #7243, #8524, #3886, #2432, #1417, #1703, #3246, #2128, #60, #8247, #3845, #5916, #7533 ) ) ;
#5166 = DIRECTION ( 'NONE',  ( 0.000000000000000000, 0.000000000000000000, 1.000000000000000000 ) ) ;
#5167 = AXIS2_PLACEMENT_3D ( 'NONE', #641, #6415, #3379 ) ;
#5168 = DIRECTION ( 'NONE',  ( 0.000000000000000000, 0.000000000000000000, 1.000000000000000000 ) ) ;
#5169 = FACE_OUTER_BOUND ( 'NONE', #2325, .T. ) ;
#5170 = CIRCLE ( 'NONE', #114, 15.00000000000000000 ) ;
#5171 = DIRECTION ( 'NONE',  ( 1.000000000000000000, 0.000000000000000000, 0.000000000000000000 ) ) ;
#5172 = CARTESIAN_POINT ( 'NONE',  ( 0.000000000000000000, 0.000000000000000000, 48.00000000000036948 ) ) ;
#5173 = AXIS2_PLACEMENT_3D ( 'NONE', #1840, #7554, #2422 ) ;
#5174 = EDGE_LOOP ( 'NONE', ( #6242, #4103, #6139, #7067, #4178 ) ) ;
#5175 = EDGE_LOOP ( 'NONE', ( #5162, #8623 ) ) ;
#5176 = DIRECTION ( 'NONE',  ( 0.000000000000000000, -1.000000000000000000, 0.000000000000000000 ) ) ;
#5177 = CARTESIAN_POINT ( 'NONE',  ( 12.37436867076458036, 12.37436867076458036, 44.37436867076458213 ) ) ;
#5178 = ORIENTED_EDGE ( 'NONE', *, *, #6593, .F. ) ;
#5179 = CIRCLE ( 'NONE', #1038, 18.50000000000000355 ) ;
#5180 = CARTESIAN_POINT ( 'NONE',  ( -0.3423334138323023135, 28.74982858564768762, 1.749889805059230419 ) ) ;
#5181 = AXIS2_PLACEMENT_3D ( 'NONE', #3220, #6783, #6741 ) ;
#5182 = ADVANCED_FACE ( 'NONE', ( #519 ), #1920, .T. ) ;
#5183 = VECTOR ( 'NONE', #5226, 1000.000000000000000 ) ;
#5184 = DIRECTION ( 'NONE',  ( 0.000000000000000000, 0.000000000000000000, 1.000000000000000000 ) ) ;
#5185 = FACE_OUTER_BOUND ( 'NONE', #1136, .T. ) ;
#5186 = ORIENTED_EDGE ( 'NONE', *, *, #6271, .F. ) ;
#5187 = ORIENTED_EDGE ( 'NONE', *, *, #2347, .F. ) ;
#5188 = DIRECTION ( 'NONE',  ( 1.864827736675067626E-17, -0.9997175446104179519, 0.02376617340079652599 ) ) ;
#5189 = ORIENTED_EDGE ( 'NONE', *, *, #427, .F. ) ;
#5190 = LINE ( 'NONE', #4374, #959 ) ;
#5191 = AXIS2_PLACEMENT_3D ( 'NONE', #787, #3628, #5988 ) ;
#5192 = CARTESIAN_POINT ( 'NONE',  ( -22.50000000000000355, 0.000000000000000000, 10.00000000000000000 ) ) ;
#5193 = VECTOR ( 'NONE', #5688, 1000.000000000000000 ) ;
#5194 = B_SPLINE_CURVE_WITH_KNOTS ( 'NONE', 3,
 ( #3777, #6146, #1805, #8387, #6719, #2346, #5994, #9058, #6859, #2393, #9011, #6042, #2532, #8962 ),
 .UNSPECIFIED., .F., .F.,
 ( 4, 2, 2, 2, 2, 2, 4 ),
 ( 0.008014353914675810889, 0.01001537843003028581, 0.01101589068770752328, 0.01201640294538476247, 0.01301691520306200167, 0.01401742746073924087, 0.01601845197609371926 ),
 .UNSPECIFIED. ) ;
#5195 = FACE_OUTER_BOUND ( 'NONE', #2812, .T. ) ;
#5196 = CARTESIAN_POINT ( 'NONE',  ( 26.02777777777776436, -7.180166011355007427, 0.000000000000000000 ) ) ;
#5197 = DIRECTION ( 'NONE',  ( 1.000000000000000000, -0.000000000000000000, -0.000000000000000000 ) ) ;
#5198 = CARTESIAN_POINT ( 'NONE',  ( 37.00000000000000000, -30.00000000000000000, -13.00000000000001066 ) ) ;
#5199 = CIRCLE ( 'NONE', #1201, 0.7499999999989250821 ) ;
#5200 = VERTEX_POINT ( 'NONE', #2651 ) ;
#5201 = VECTOR ( 'NONE', #926, 1000.000000000000000 ) ;
#5202 = PRESENTATION_STYLE_ASSIGNMENT (( #2471 ) ) ;
#5203 = EDGE_LOOP ( 'NONE', ( #2676, #6036, #8389, #8295 ) ) ;
#5204 = PLANE ( 'NONE',  #1574 ) ;
#5205 = DIRECTION ( 'NONE',  ( 1.000000000000000000, 0.000000000000000000, 0.000000000000000000 ) ) ;
#5206 = CARTESIAN_POINT ( 'NONE',  ( 12.37436867076458036, 12.37436867076458036, 44.37436867076458213 ) ) ;
#5207 = DIRECTION ( 'NONE',  ( 1.000000000000000000, 0.000000000000000000, 0.000000000000000000 ) ) ;
#5208 = ORIENTED_EDGE ( 'NONE', *, *, #6651, .T. ) ;
#5209 = EDGE_LOOP ( 'NONE', ( #6848, #8598, #4467, #6349 ) ) ;
#5210 = VERTEX_POINT ( 'NONE', #6619 ) ;
#5211 =( LENGTH_UNIT ( ) NAMED_UNIT ( * ) SI_UNIT ( .MILLI., .METRE. ) );
#5212 = EDGE_LOOP ( 'NONE', ( #9205, #2535, #7010, #6110 ) ) ;
#5213 = EDGE_CURVE ( 'NONE', #5549, #9261, #3910, .T. ) ;
#5214 = DIRECTION ( 'NONE',  ( 1.000000000000000000, 0.000000000000000000, 0.000000000000000000 ) ) ;
#5215 = CARTESIAN_POINT ( 'NONE',  ( 2.143131898507868248E-15, 17.50000000000000000, 14.49999999999999822 ) ) ;
#5216 = AXIS2_PLACEMENT_3D ( 'NONE', #101, #8077, #2364 ) ;
#5217 = DIRECTION ( 'NONE',  ( 0.000000000000000000, -0.7071067811865479058, 0.7071067811865472397 ) ) ;
#5218 = DIRECTION ( 'NONE',  ( 0.000000000000000000, 0.000000000000000000, 1.000000000000000000 ) ) ;
#5219 = EDGE_CURVE ( 'NONE', #3742, #662, #994, .T. ) ;
#5220 = CARTESIAN_POINT ( 'NONE',  ( 5.000000000000000888, 0.000000000000000000, 4.000000000000000000 ) ) ;
#5221 = LINE ( 'NONE', #8869, #2685 ) ;
#5222 = DIRECTION ( 'NONE',  ( 0.000000000000000000, 0.000000000000000000, 1.000000000000000000 ) ) ;
#5223 = EDGE_LOOP ( 'NONE', ( #2219, #5887, #1868, #5525 ) ) ;
#5224 = ORIENTED_EDGE ( 'NONE', *, *, #6338, .T. ) ;
#5225 = DIRECTION ( 'NONE',  ( 0.7071067811865463515, 0.5000000000000006661, 0.5000000000000012212 ) ) ;
#5226 = DIRECTION ( 'NONE',  ( -0.000000000000000000, -0.000000000000000000, -1.000000000000000000 ) ) ;
#5227 = ORIENTED_EDGE ( 'NONE', *, *, #7020, .F. ) ;
#5228 = EDGE_CURVE ( 'NONE', #3211, #6868, #7829, .T. ) ;
#5229 = CARTESIAN_POINT ( 'NONE',  ( 3.288881746422226193, 28.22045692612880075, 1.409579452511374065 ) ) ;
#5230 = AXIS2_PLACEMENT_3D ( 'NONE', #4354, #5710, #5800 ) ;
#5231 = CARTESIAN_POINT ( 'NONE',  ( 37.00000000000000000, -13.96446609406729067, -95.00000000000000000 ) ) ;
#5232 =( REPRESENTATION_RELATIONSHIP ('NONE','NONE', #1933, #8501 ) REPRESENTATION_RELATIONSHIP_WITH_TRANSFORMATION ( #7972 )SHAPE_REPRESENTATION_RELATIONSHIP( ) );
#5233 = CARTESIAN_POINT ( 'NONE',  ( 0.000000000000000000, 18.47759065022580316, -6.903668647301629768 ) ) ;
#5234 = ORIENTED_EDGE ( 'NONE', *, *, #3359, .T. ) ;
#5235 = VERTEX_POINT ( 'NONE', #4175 ) ;
#5236 = PRODUCT_CONTEXT ( 'NONE', #1981, 'mechanical' ) ;
#5237 = ADVANCED_FACE ( 'NONE', ( #8773 ), #4898, .F. ) ;
#5238 = EDGE_CURVE ( 'NONE', #3697, #1904, #3447, .T. ) ;
#5239 = DIRECTION ( 'NONE',  ( -1.000000000000000000, -0.000000000000000000, -0.000000000000000000 ) ) ;
#5240 = CARTESIAN_POINT ( 'NONE',  ( 0.7500000000000000000, -0.7500000000000000000, 1.500000000000000000 ) ) ;
#5241 = ADVANCED_FACE ( 'NONE', ( #8050 ), #3682, .F. ) ;
#5242 = EDGE_CURVE ( 'NONE', #7405, #3020, #2746, .T. ) ;
#5243 = EDGE_CURVE ( 'NONE', #4363, #9426, #2210, .T. ) ;
#5244 = VECTOR ( 'NONE', #8472, 1000.000000000000000 ) ;
#5245 = DIRECTION ( 'NONE',  ( -1.000000000000000000, 0.000000000000000000, 0.000000000000000000 ) ) ;
#5246 = CARTESIAN_POINT ( 'NONE',  ( 26.21170834203229916, -53.97171801779367684, 11.99999999999999645 ) ) ;
#5247 = CYLINDRICAL_SURFACE ( 'NONE', #447, 1.560000000001265263 ) ;
#5248 = DIRECTION ( 'NONE',  ( 0.000000000000000000, 0.000000000000000000, -1.000000000000000000 ) ) ;
#5249 = CARTESIAN_POINT ( 'NONE',  ( 3.168636005459071203, -27.60958896060100543, 0.7887504010224316575 ) ) ;
#5250 =( BOUNDED_CURVE ( )  B_SPLINE_CURVE ( 3, ( #9192, #4742, #1855, #8386 ),
 .UNSPECIFIED., .F., .F. ) 
 B_SPLINE_CURVE_WITH_KNOTS ( ( 4, 4 ),
 ( 5.235987755982988823, 5.613918313269388172 ),
 .UNSPECIFIED. ) 
 CURVE ( )  GEOMETRIC_REPRESENTATION_ITEM ( )  RATIONAL_B_SPLINE_CURVE ( ( 1.000000000000000000, 0.9881327504826167285, 0.9881327504826167285, 1.000000000000000000 ) ) 
 REPRESENTATION_ITEM ( '' )  );
#5251 = ORIENTED_EDGE ( 'NONE', *, *, #3518, .T. ) ;
#5252 = EDGE_LOOP ( 'NONE', ( #219, #5644, #6592, #2407 ) ) ;
#5253 = AXIS2_PLACEMENT_3D ( 'NONE', #205, #5821, #4040 ) ;
#5254 = PLANE ( 'NONE',  #9389 ) ;
#5255 = DIRECTION ( 'NONE',  ( -1.000000000000000000, -0.000000000000000000, -0.000000000000000000 ) ) ;
#5256 = ADVANCED_FACE ( 'NONE', ( #4399 ), #2190, .F. ) ;
#5257 = VECTOR ( 'NONE', #6025, 1000.000000000000000 ) ;
#5258 = ADVANCED_FACE ( 'NONE', ( #7148 ), #4084, .F. ) ;
#5259 = DIRECTION ( 'NONE',  ( 0.000000000000000000, 0.000000000000000000, -1.000000000000000000 ) ) ;
#5260 = LINE ( 'NONE', #5156, #3862 ) ;
#5261 = EDGE_CURVE ( 'NONE', #1522, #1000, #5605, .T. ) ;
#5262 = ORIENTED_EDGE ( 'NONE', *, *, #8639, .F. ) ;
#5263 = EDGE_LOOP ( 'NONE', ( #7297, #8211, #9013, #8649 ) ) ;
#5264 = EDGE_LOOP ( 'NONE', ( #6351, #5454, #3343, #6399, #449, #9091 ) ) ;
#5265 = FILL_AREA_STYLE_COLOUR ( '', #7778 ) ;
#5266 = AXIS2_PLACEMENT_3D ( 'NONE', #820, #4526, #1401 ) ;
#5267 = VERTEX_POINT ( 'NONE', #750 ) ;
#5268 = DIRECTION ( 'NONE',  ( -1.000000000000000000, 0.000000000000000000, 0.000000000000000000 ) ) ;
#5269 = DIRECTION ( 'NONE',  ( 0.000000000000000000, 0.000000000000000000, 1.000000000000000000 ) ) ;
#5270 = DIRECTION ( 'NONE',  ( -1.000000000000000000, 0.000000000000000000, 0.000000000000000000 ) ) ;
#5271 = DIRECTION ( 'NONE',  ( 0.000000000000000000, 0.000000000000000000, 1.000000000000000000 ) ) ;
#5272 = DIRECTION ( 'NONE',  ( -0.000000000000000000, -0.000000000000000000, -1.000000000000000000 ) ) ;
#5273 = AXIS2_PLACEMENT_3D ( 'NONE', #3621, #6470, #208 ) ;
#5274 = CARTESIAN_POINT ( 'NONE',  ( -31.99999999999999289, 2.265596578422605368E-15, 13.49999999999998401 ) ) ;
#5275 = CARTESIAN_POINT ( 'NONE',  ( -0.7500000000000000000, 0.7500000000000000000, 0.000000000000000000 ) ) ;
#5276 = ORIENTED_EDGE ( 'NONE', *, *, #6305, .T. ) ;
#5277 = ORIENTED_EDGE ( 'NONE', *, *, #2068, .F. ) ;
#5278 = DIRECTION ( 'NONE',  ( -1.000000000000000000, 0.000000000000000000, 0.000000000000000000 ) ) ;
#5279 = ORIENTED_EDGE ( 'NONE', *, *, #8541, .T. ) ;
#5280 = CONICAL_SURFACE ( 'NONE', #8188, 17.50000000000000355, 0.7853981633974466137 ) ;
#5281 = DIRECTION ( 'NONE',  ( -1.000000000000000000, 0.000000000000000000, 0.000000000000000000 ) ) ;
#5282 = AXIS2_PLACEMENT_3D ( 'NONE', #3648, #8924, #9452 ) ;
#5283 = DIRECTION ( 'NONE',  ( 0.000000000000000000, 1.000000000000000000, 0.000000000000000000 ) ) ;
#5284 = UNCERTAINTY_MEASURE_WITH_UNIT (LENGTH_MEASURE( 1.000000000000000082E-05 ), #2436, 'distance_accuracy_value', 'NONE');
#5285 = FACE_OUTER_BOUND ( 'NONE', #4734, .T. ) ;
#5286 = ORIENTED_EDGE ( 'NONE', *, *, #913, .T. ) ;
#5287 = ORIENTED_EDGE ( 'NONE', *, *, #4829, .T. ) ;
#5288 = CIRCLE ( 'NONE', #1445, 2.999999999999999112 ) ;
#5289 = CARTESIAN_POINT ( 'NONE',  ( 16.00000000000000000, 43.00000000000000000, 11.99999999999999645 ) ) ;
#5290 = CARTESIAN_POINT ( 'NONE',  ( 0.000000000000000000, -14.14213562373248401, -15.70213562373165850 ) ) ;
#5291 = AXIS2_PLACEMENT_3D ( 'NONE', #7267, #6469, #9281 ) ;
#5292 =( REPRESENTATION_RELATIONSHIP ('NONE','NONE', #1933, #6298 ) REPRESENTATION_RELATIONSHIP_WITH_TRANSFORMATION ( #1871 )SHAPE_REPRESENTATION_RELATIONSHIP( ) );
#5293 = DIRECTION ( 'NONE',  ( 1.000000000000000000, 0.000000000000000000, 0.000000000000000000 ) ) ;
#5294 = DIRECTION ( 'NONE',  ( -1.000000000000000000, 0.000000000000000000, 0.000000000000000000 ) ) ;
#5295 = CARTESIAN_POINT ( 'NONE',  ( -0.7500000000000000000, -0.7500000000000000000, 1.500000000000000000 ) ) ;
#5296 = DIRECTION ( 'NONE',  ( -1.000000000000000000, 0.000000000000000000, 0.000000000000000000 ) ) ;
#5297 = CARTESIAN_POINT ( 'NONE',  ( -0.8460976106426699728, -28.45495154861555065, 1.464499174736009879 ) ) ;
#5298 = ORIENTED_EDGE ( 'NONE', *, *, #137, .F. ) ;
#5299 = EDGE_CURVE ( 'NONE', #8340, #2574, #41, .T. ) ;
#5300 = SURFACE_STYLE_USAGE ( .BOTH. , #9038 ) ;
#5301 = ADVANCED_FACE ( 'NONE', ( #6345 ), #1667, .T. ) ;
#5302 = ORIENTED_EDGE ( 'NONE', *, *, #8911, .F. ) ;
#5303 = DIRECTION ( 'NONE',  ( 0.000000000000000000, 0.7071067811865479058, -0.7071067811865472397 ) ) ;
#5304 = DIRECTION ( 'NONE',  ( 1.000000000000000000, 0.000000000000000000, 0.000000000000000000 ) ) ;
#5305 = AXIS2_PLACEMENT_3D ( 'NONE', #7813, #1222, #7087 ) ;
#5306 = CARTESIAN_POINT ( 'NONE',  ( 4.000000000000000000, 9.603694566548697359E-13, 21.56000000000303984 ) ) ;
#5307 = DIRECTION ( 'NONE',  ( -1.000000000000000000, 0.000000000000000000, 0.000000000000000000 ) ) ;
#5308 = ORIENTED_EDGE ( 'NONE', *, *, #6671, .T. ) ;
#5309 = VERTEX_POINT ( 'NONE', #6664 ) ;
#5310 = AXIS2_PLACEMENT_3D ( 'NONE', #7542, #3077, #3791 ) ;
#5311 = ORIENTED_EDGE ( 'NONE', *, *, #3408, .T. ) ;
#5312 = ORIENTED_EDGE ( 'NONE', *, *, #1009, .F. ) ;
#5313 = DIRECTION ( 'NONE',  ( 0.000000000000000000, 0.000000000000000000, 1.000000000000000000 ) ) ;
#5314 = CARTESIAN_POINT ( 'NONE',  ( -0.7500000000000000000, -0.7500000000000000000, 0.000000000000000000 ) ) ;
#5315 = EDGE_CURVE ( 'NONE', #5682, #1677, #6824, .T. ) ;
#5316 = CARTESIAN_POINT ( 'NONE',  ( 17.50000000000000355, 0.000000000000000000, 0.000000000000000000 ) ) ;
#5317 = CARTESIAN_POINT ( 'NONE',  ( 22.50000000000000355, 0.000000000000000000, 0.000000000000000000 ) ) ;
#5318 = VECTOR ( 'NONE', #960, 1000.000000000000000 ) ;
#5319 = CARTESIAN_POINT ( 'NONE',  ( 22.50000000000000355, 2.356749903719115078E-13, 5.000000000000000000 ) ) ;
#5320 = ADVANCED_FACE ( 'NONE', ( #8106 ), #790, .T. ) ;
#5321 = CARTESIAN_POINT ( 'NONE',  ( 38.00000000000000000, -43.00000000000000000, 11.99999999999999645 ) ) ;
#5322 = CARTESIAN_POINT ( 'NONE',  ( -22.50000000000000000, -7.855833012397050680E-14, 15.00000000000000000 ) ) ;
#5323 = VERTEX_POINT ( 'NONE', #9007 ) ;
#5324 = ORIENTED_EDGE ( 'NONE', *, *, #5023, .F. ) ;
#5325 = CYLINDRICAL_SURFACE ( 'NONE', #3607, 3.000000000000002665 ) ;
#5326 = ORIENTED_EDGE ( 'NONE', *, *, #4812, .F. ) ;
#5327 = VECTOR ( 'NONE', #4689, 1000.000000000000000 ) ;
#5328 = CARTESIAN_POINT ( 'NONE',  ( 0.000000000000000000, 0.000000000000000000, 10.00000000000000000 ) ) ;
#5329 = CARTESIAN_POINT ( 'NONE',  ( 0.000000000000000000, 0.000000000000000000, 0.000000000000000000 ) ) ;
#5330 = VECTOR ( 'NONE', #9288, 1000.000000000000000 ) ;
#5331 = VERTEX_POINT ( 'NONE', #2291 ) ;
#5332 = DIRECTION ( 'NONE',  ( 0.000000000000000000, 0.000000000000000000, -1.000000000000000000 ) ) ;
#5333 = VECTOR ( 'NONE', #8032, 999.9999999999998863 ) ;
#5334 = AXIS2_PLACEMENT_3D ( 'NONE', #7990, #5255, #5062 ) ;
#5335 = CARTESIAN_POINT ( 'NONE',  ( 0.000000000000000000, 0.000000000000000000, 13.66147716702868031 ) ) ;
#5336 = DIRECTION ( 'NONE',  ( 0.000000000000000000, 0.000000000000000000, 1.000000000000000000 ) ) ;
#5337 = AXIS2_PLACEMENT_3D ( 'NONE', #2344, #8248, #9057 ) ;
#5338 = ORIENTED_EDGE ( 'NONE', *, *, #4009, .F. ) ;
#5339 = ORIENTED_EDGE ( 'NONE', *, *, #3502, .T. ) ;
#5340 = DIRECTION ( 'NONE',  ( 0.9994148367277968514, 0.0008129226918946572296, 0.03419536935095434521 ) ) ;
#5341 = AXIS2_PLACEMENT_3D ( 'NONE', #3543, #9404, #6931 ) ;
#5342 = EDGE_CURVE ( 'NONE', #956, #1434, #2381, .T. ) ;
#5343 = VECTOR ( 'NONE', #8310, 1000.000000000000000 ) ;
#5344 = CARTESIAN_POINT ( 'NONE',  ( 37.22467645238197775, 47.05659850664388699, -0.5000000000000038858 ) ) ;
#5345 = CARTESIAN_POINT ( 'NONE',  ( -31.99999999999999289, -29.99999999999996447, 5.000000000000005329 ) ) ;
#5346 = VECTOR ( 'NONE', #8206, 1000.000000000000114 ) ;
#5347 = CYLINDRICAL_SURFACE ( 'NONE', #2986, 1.560000000001265263 ) ;
#5348 = EDGE_CURVE ( 'NONE', #694, #7436, #8351, .T. ) ;
#5349 = DIRECTION ( 'NONE',  ( 0.000000000000000000, 0.000000000000000000, 1.000000000000000000 ) ) ;
#5350 = CYLINDRICAL_SURFACE ( 'NONE', #6111, 0.7500000000001915135 ) ;
#5351 = CARTESIAN_POINT ( 'NONE',  ( -28.40858913551337750, 2.655051044735472487, 1.530521587115753812 ) ) ;
#5352 = ORIENTED_EDGE ( 'NONE', *, *, #6134, .T. ) ;
#5353 = DIRECTION ( 'NONE',  ( 0.000000000000000000, 0.000000000000000000, -1.000000000000000000 ) ) ;
#5354 = VECTOR ( 'NONE', #1370, 1000.000000000000114 ) ;
#5355 = ORIENTED_EDGE ( 'NONE', *, *, #657, .F. ) ;
#5356 = DIRECTION ( 'NONE',  ( 0.000000000000000000, -0.000000000000000000, 1.000000000000000000 ) ) ;
#5357 = DIRECTION ( 'NONE',  ( 0.000000000000000000, 0.000000000000000000, 1.000000000000000000 ) ) ;
#5358 = FACE_OUTER_BOUND ( 'NONE', #9240, .T. ) ;
#5359 = DIRECTION ( 'NONE',  ( 0.000000000000000000, 0.000000000000000000, 1.000000000000000000 ) ) ;
#5360 = VECTOR ( 'NONE', #1179, 1000.000000000000000 ) ;
#5361 = AXIS2_PLACEMENT_3D ( 'NONE', #2073, #5002, #3560 ) ;
#5362 = ORIENTED_EDGE ( 'NONE', *, *, #2604, .T. ) ;
#5363 = EDGE_LOOP ( 'NONE', ( #9045, #9071, #2494, #6183 ) ) ;
#5364 = ORIENTED_EDGE ( 'NONE', *, *, #3536, .T. ) ;
#5365 = SHAPE_REPRESENTATION_RELATIONSHIP ( 'NONE' , 'NONE' ,  #6964, #7497 ) ;
#5366 = ORIENTED_EDGE ( 'NONE', *, *, #8658, .T. ) ;
#5367 = LINE ( 'NONE', #221, #140 ) ;
#5368 = EDGE_CURVE ( 'NONE', #2936, #1890, #6232, .T. ) ;
#5369 = DIRECTION ( 'NONE',  ( -0.6785983445458484420, -0.2810846377148113473, -0.6785983445458493302 ) ) ;
#5370 = VECTOR ( 'NONE', #2981, 1000.000000000000000 ) ;
#5371 = EDGE_CURVE ( 'NONE', #3861, #8166, #8912, .T. ) ;
#5372 = FACE_BOUND ( 'NONE', #740, .T. ) ;
#5373 = DIRECTION ( 'NONE',  ( -0.000000000000000000, -0.000000000000000000, -1.000000000000000000 ) ) ;
#5374 = DIRECTION ( 'NONE',  ( 0.000000000000000000, 0.000000000000000000, -1.000000000000000000 ) ) ;
#5375 = CARTESIAN_POINT ( 'NONE',  ( 37.00000000000000000, -8.017766952966344007, -116.9822330470336453 ) ) ;
#5376 = CARTESIAN_POINT ( 'NONE',  ( 37.00000000000000000, 15.90990257669733943, -54.09009742330271564 ) ) ;
#5377 = ORIENTED_EDGE ( 'NONE', *, *, #2249, .T. ) ;
#5378 = ORIENTED_EDGE ( 'NONE', *, *, #6250, .F. ) ;
#5379 = CARTESIAN_POINT ( 'NONE',  ( 0.000000000000000000, 22.50000000000000355, 10.00000000000000000 ) ) ;
#5380 = VERTEX_POINT ( 'NONE', #226 ) ;
#5381 = CARTESIAN_POINT ( 'NONE',  ( 0.000000000000000000, 0.000000000000000000, 10.00000000000000000 ) ) ;
#5382 = CARTESIAN_POINT ( 'NONE',  ( 0.000000000000000000, -29.99999999999999289, 64.00000000000000000 ) ) ;
#5383 = EDGE_LOOP ( 'NONE', ( #755, #8535, #2984, #9126, #5685, #9286, #923, #7225, #1630, #5646, #6987, #5311, #6678, #1245, #8569, #718, #9199, #8659, #1303, #8900 ) ) ;
#5384 = CARTESIAN_POINT ( 'NONE',  ( 5.088821267330767562, 27.44505377838575200, 0.9111060003908462157 ) ) ;
#5385 = DIRECTION ( 'NONE',  ( 0.000000000000000000, 0.000000000000000000, -1.000000000000000000 ) ) ;
#5386 = CARTESIAN_POINT ( 'NONE',  ( -3.288881746422226193, -28.22045692612880075, 1.409579452511374065 ) ) ;
#5387 = EDGE_LOOP ( 'NONE', ( #3075, #5518, #7065, #7726, #9147, #541, #9227, #6811 ) ) ;
#5388 = ORIENTED_EDGE ( 'NONE', *, *, #144, .F. ) ;
#5389 = CONTEXT_DEPENDENT_SHAPE_REPRESENTATION ( #5102, #707 ) ;
#5390 = CARTESIAN_POINT ( 'NONE',  ( 31.00000000000002132, 2.143131898507869037E-15, 49.50000000000000000 ) ) ;
#5391 = DIRECTION ( 'NONE',  ( 0.000000000000000000, 0.000000000000000000, 1.000000000000000000 ) ) ;
#5392 = CARTESIAN_POINT ( 'NONE',  ( 53.29490495164537833, -1.836970198721028011E-15, -85.00000000000000000 ) ) ;
#5393 =( LENGTH_UNIT ( ) NAMED_UNIT ( * ) SI_UNIT ( .MILLI., .METRE. ) );
#5394 = DIRECTION ( 'NONE',  ( 0.7071067811865439090, 8.659560562354888485E-17, -0.7071067811865511255 ) ) ;
#5395 = DIRECTION ( 'NONE',  ( 1.000000000000000000, 0.000000000000000000, 0.000000000000000000 ) ) ;
#5396 = AXIS2_PLACEMENT_3D ( 'NONE', #9191, #2628, #5558 ) ;
#5397 = ORIENTED_EDGE ( 'NONE', *, *, #8229, .F. ) ;
#5398 = ORIENTED_EDGE ( 'NONE', *, *, #6218, .T. ) ;
#5399 = CARTESIAN_POINT ( 'NONE',  ( 27.00000000000000355, -34.99999999999999289, 64.00000000000000000 ) ) ;
#5400 = PLANE ( 'NONE',  #3016 ) ;
#5401 = DIRECTION ( 'NONE',  ( -1.000000000000000000, -0.000000000000000000, -0.000000000000000000 ) ) ;
#5402 = CARTESIAN_POINT ( 'NONE',  ( 27.00000000000000000, -43.00000000000000000, 11.99999999999999645 ) ) ;
#5403 = ORIENTED_EDGE ( 'NONE', *, *, #3709, .F. ) ;
#5404 = AXIS2_PLACEMENT_3D ( 'NONE', #6609, #393, #3908 ) ;
#5405 = ORIENTED_EDGE ( 'NONE', *, *, #4597, .F. ) ;
#5406 = ORIENTED_EDGE ( 'NONE', *, *, #6729, .T. ) ;
#5407 = EDGE_LOOP ( 'NONE', ( #6471, #6988 ) ) ;
#5408 = CARTESIAN_POINT ( 'NONE',  ( -28.50000000000000000, -7.855833971761515132E-14, 1.500000000000037748 ) ) ;
#5409 = DIRECTION ( 'NONE',  ( 0.5773502691896285066, 0.5773502691896228445, -0.5773502691896261751 ) ) ;
#5410 = FACE_OUTER_BOUND ( 'NONE', #2722, .T. ) ;
#5411 = CARTESIAN_POINT ( 'NONE',  ( 0.000000000000000000, 34.00000000000001421, 32.00000000000000000 ) ) ;
#5412 = CARTESIAN_POINT ( 'NONE',  ( 0.000000000000000000, 0.000000000000000000, 11.00000000000000000 ) ) ;
#5413 = CIRCLE ( 'NONE', #8481, 0.7500000000013675727 ) ;
#5414 = CARTESIAN_POINT ( 'NONE',  ( 3.000000000000000000, 22.50000000000000355, 10.00000000000000000 ) ) ;
#5415 = ORIENTED_EDGE ( 'NONE', *, *, #5960, .F. ) ;
#5416 = EDGE_CURVE ( 'NONE', #6441, #5921, #3872, .T. ) ;
#5417 = VERTEX_POINT ( 'NONE', #7521 ) ;
#5418 = CARTESIAN_POINT ( 'NONE',  ( -22.50000000000000000, -7.855833012397050680E-14, 0.000000000000000000 ) ) ;
#5419 = VERTEX_POINT ( 'NONE', #940 ) ;
#5420 = ADVANCED_FACE ( 'NONE', ( #4547, #6091 ), #2390, .F. ) ;
#5421 = FACE_BOUND ( 'NONE', #6223, .T. ) ;
#5422 = DIRECTION ( 'NONE',  ( -1.000000000000000000, 0.000000000000000000, 0.000000000000000000 ) ) ;
#5423 = EDGE_CURVE ( 'NONE', #3262, #2860, #8511, .T. ) ;
#5424 = EDGE_CURVE ( 'NONE', #1561, #472, #4515, .T. ) ;
#5425 = ORIENTED_EDGE ( 'NONE', *, *, #7216, .F. ) ;
#5426 =( REPRESENTATION_RELATIONSHIP ('NONE','NONE', #1933, #8501 ) REPRESENTATION_RELATIONSHIP_WITH_TRANSFORMATION ( #566 )SHAPE_REPRESENTATION_RELATIONSHIP( ) );
#5427 = LINE ( 'NONE', #6245, #8707 ) ;
#5428 = CYLINDRICAL_SURFACE ( 'NONE', #7581, 30.00000000000000000 ) ;
#5429 = CARTESIAN_POINT ( 'NONE',  ( -3.600085285568724203, -28.11218154377481682, 1.339973849569531472 ) ) ;
#5430 = ORIENTED_EDGE ( 'NONE', *, *, #6530, .T. ) ;
#5431 = ADVANCED_BREP_SHAPE_REPRESENTATION ( '', ( #6309, #1614 ), #4537 ) ;
#5432 = ORIENTED_EDGE ( 'NONE', *, *, #9144, .T. ) ;
#5433 = AXIS2_PLACEMENT_3D ( 'NONE', #6952, #362, #457 ) ;
#5434 = CONTEXT_DEPENDENT_SHAPE_REPRESENTATION ( #5292, #8921 ) ;
#5435 = ADVANCED_FACE ( 'NONE', ( #5939 ), #236, .T. ) ;
#5436 = LINE ( 'NONE', #202, #5343 ) ;
#5437 = CARTESIAN_POINT ( 'NONE',  ( -19.50000000000000000, -7.819093608422630136E-14, 10.00000000000000000 ) ) ;
#5438 = CARTESIAN_POINT ( 'NONE',  ( 60.00000000000000000, -15.90990257669733943, -85.90990257669729147 ) ) ;
#5439 = DIRECTION ( 'NONE',  ( -0.000000000000000000, -1.000000000000000000, -0.000000000000000000 ) ) ;
#5440 = EDGE_CURVE ( 'NONE', #2461, #4466, #2302, .T. ) ;
#5441 = CARTESIAN_POINT ( 'NONE',  ( 2.143131898507868248E-15, -35.00000000000000000, 14.49999999999999822 ) ) ;
#5442 = ORIENTED_EDGE ( 'NONE', *, *, #308, .T. ) ;
#5443 = AXIS2_PLACEMENT_3D ( 'NONE', #240, #8452, #4561 ) ;
#5444 = CARTESIAN_POINT ( 'NONE',  ( 37.00000000000000000, -15.90990257669733943, -51.09009742330271564 ) ) ;
#5445 = ORIENTED_EDGE ( 'NONE', *, *, #4142, .F. ) ;
#5446 = CARTESIAN_POINT ( 'NONE',  ( -26.21170834203229205, -53.97171801779368394, 11.99999999999999645 ) ) ;
#5447 = AXIS2_PLACEMENT_3D ( 'NONE', #3619, #5700, #3472 ) ;
#5448 = CARTESIAN_POINT ( 'NONE',  ( 37.00000000000000000, 30.00000000000000000, -95.00000000000000000 ) ) ;
#5449 = CARTESIAN_POINT ( 'NONE',  ( 16.00000000000000000, 0.000000000000000000, 9.999999999999998224 ) ) ;
#5450 = CARTESIAN_POINT ( 'NONE',  ( 5.000000000000000000, -14.14213562373112154, 12.58213562373271621 ) ) ;
#5451 = ORIENTED_EDGE ( 'NONE', *, *, #6846, .T. ) ;
#5452 = AXIS2_PLACEMENT_3D ( 'NONE', #4039, #7591, #3221 ) ;
#5453 = ORIENTED_EDGE ( 'NONE', *, *, #8909, .T. ) ;
#5454 = ORIENTED_EDGE ( 'NONE', *, *, #6266, .F. ) ;
#5455 = ORIENTED_EDGE ( 'NONE', *, *, #1752, .F. ) ;
#5456 = CARTESIAN_POINT ( 'NONE',  ( 60.00000000000000000, 7.347880794884118356E-15, -30.00000000000000000 ) ) ;
#5457 = FACE_OUTER_BOUND ( 'NONE', #1263, .T. ) ;
#5458 = CARTESIAN_POINT ( 'NONE',  ( -53.29490495164537833, 11.46446609406724626, -97.50000000000000000 ) ) ;
#5459 = ADVANCED_FACE ( 'NONE', ( #5169 ), #1755, .T. ) ;
#5460 = DIRECTION ( 'NONE',  ( -0.000000000000000000, -0.000000000000000000, 1.000000000000000000 ) ) ;
#5461 = DIRECTION ( 'NONE',  ( 1.000000000000000000, 0.000000000000000000, 0.000000000000000000 ) ) ;
#5462 = CARTESIAN_POINT ( 'NONE',  ( 0.000000000000000000, 0.000000000000000000, 8.000000000000005329 ) ) ;
#5463 = EDGE_CURVE ( 'NONE', #6611, #3327, #7429, .T. ) ;
#5464 = LINE ( 'NONE', #7474, #812 ) ;
#5465 = VERTEX_POINT ( 'NONE', #3061 ) ;
#5466 = ORIENTED_EDGE ( 'NONE', *, *, #2717, .T. ) ;
#5467 = DIRECTION ( 'NONE',  ( -1.000000000000000000, 0.000000000000000000, 0.000000000000000000 ) ) ;
#5468 = ORIENTED_EDGE ( 'NONE', *, *, #1426, .F. ) ;
#5469 = FACE_OUTER_BOUND ( 'NONE', #86, .T. ) ;
#5470 = LINE ( 'NONE', #1863, #8104 ) ;
#5471 = ORIENTED_EDGE ( 'NONE', *, *, #8930, .F. ) ;
#5472 = CIRCLE ( 'NONE', #4545, 6.000000000000000888 ) ;
#5473 = DIRECTION ( 'NONE',  ( -0.000000000000000000, -0.000000000000000000, 1.000000000000000000 ) ) ;
#5474 = FACE_OUTER_BOUND ( 'NONE', #5387, .T. ) ;
#5475 = DIRECTION ( 'NONE',  ( 0.000000000000000000, 0.000000000000000000, -1.000000000000000000 ) ) ;
#5476 = VERTEX_POINT ( 'NONE', #1124 ) ;
#5477 = EDGE_LOOP ( 'NONE', ( #3841, #3249 ) ) ;
#5478 = CONTEXT_DEPENDENT_SHAPE_REPRESENTATION ( #8548, #8604 ) ;
#5479 = CLOSED_SHELL ( 'NONE', ( #7061, #8698, #8274, #3970, #2605, #2023, #6072, #8134, #6776, #6830, #4413, #714, #1237, #2743, #596, #2369, #8642, #3922, #2140, #8234, #1902, #7730, #6224, #364, #1839, #8457, #9348, #2563, #2028, #9068, #3884, #3745, #5528 ) ) ;
#5480 = DIRECTION ( 'NONE',  ( -1.000000000000000000, 0.000000000000000000, 0.000000000000000000 ) ) ;
#5481 = EDGE_CURVE ( 'NONE', #5629, #1677, #4064, .T. ) ;
#5482 = AXIS2_PLACEMENT_3D ( 'NONE', #1696, #6216, #7507 ) ;
#5483 = CARTESIAN_POINT ( 'NONE',  ( 19.00000000000000000, 0.000000000000000000, 17.50000000000000000 ) ) ;
#5484 = AXIS2_PLACEMENT_3D ( 'NONE', #6581, #4411, #2199 ) ;
#5485 =( NAMED_UNIT ( * ) SI_UNIT ( $, .STERADIAN. ) SOLID_ANGLE_UNIT ( ) );
#5486 = LINE ( 'NONE', #8417, #1332 ) ;
#5487 = AXIS2_PLACEMENT_3D ( 'NONE', #3260, #5475, #8349 ) ;
#5488 = CARTESIAN_POINT ( 'NONE',  ( -27.00000000000000000, 43.00000000000000000, -25.00000000000000000 ) ) ;
#5489 = AXIS2_PLACEMENT_3D ( 'NONE', #8684, #2100, #7971 ) ;
#5490 = EDGE_LOOP ( 'NONE', ( #6010, #6122, #5729, #6493 ) ) ;
#5491 = VECTOR ( 'NONE', #1982, 1000.000000000000000 ) ;
#5492 = PLANE ( 'NONE',  #4410 ) ;
#5493 = EDGE_LOOP ( 'NONE', ( #452, #7779 ) ) ;
#5494 = AXIS2_PLACEMENT_3D ( 'NONE', #7244, #3592, #6529 ) ;
#5495 = CARTESIAN_POINT ( 'NONE',  ( -22.50000000000000355, 0.000000000000000000, 5.000000000000000000 ) ) ;
#5496 = CYLINDRICAL_SURFACE ( 'NONE', #7016, 1.559999999999096776 ) ;
#5497 = VECTOR ( 'NONE', #1422, 1000.000000000000000 ) ;
#5498 = DIRECTION ( 'NONE',  ( 0.000000000000000000, 0.000000000000000000, 1.000000000000000000 ) ) ;
#5499 = AXIS2_PLACEMENT_3D ( 'NONE', #5579, #5530, #7737 ) ;
#5500 = LINE ( 'NONE', #1743, #1247 ) ;
#5501 = CIRCLE ( 'NONE', #734, 1.000000000000000000 ) ;
#5502 = EDGE_LOOP ( 'NONE', ( #8876, #3133, #3111, #3159, #5324 ) ) ;
#5503 = ORIENTED_EDGE ( 'NONE', *, *, #6602, .F. ) ;
#5504 = DIRECTION ( 'NONE',  ( 0.000000000000000000, 0.000000000000000000, 1.000000000000000000 ) ) ;
#5505 = VERTEX_POINT ( 'NONE', #7759 ) ;
#5506 = CARTESIAN_POINT ( 'NONE',  ( 53.29490495164537833, -15.90990257669733943, -57.09009742330271564 ) ) ;
#5507 = CARTESIAN_POINT ( 'NONE',  ( -53.29490495164537833, -30.00000000000000000, -97.50000000000000000 ) ) ;
#5508 = AXIS2_PLACEMENT_3D ( 'NONE', #4491, #836, #3770 ) ;
#5509 = CIRCLE ( 'NONE', #6740, 1.559999999999096776 ) ;
#5510 = LINE ( 'NONE', #9333, #7689 ) ;
#5511 = CIRCLE ( 'NONE', #6452, 1.559999999998939346 ) ;
#5512 = CARTESIAN_POINT ( 'NONE',  ( -17.49999999999999645, -4.703319286132083832, 49.50000000000000000 ) ) ;
#5513 = LINE ( 'NONE', #1219, #9410 ) ;
#5514 = EDGE_LOOP ( 'NONE', ( #8648, #5150, #5910, #8942 ) ) ;
#5515 = VERTEX_POINT ( 'NONE', #6992 ) ;
#5516 = FACE_OUTER_BOUND ( 'NONE', #9285, .T. ) ;
#5517 = CIRCLE ( 'NONE', #3360, 6.000000000000000888 ) ;
#5518 = ORIENTED_EDGE ( 'NONE', *, *, #3163, .T. ) ;
#5519 = CARTESIAN_POINT ( 'NONE',  ( -50.79490495164537833, -30.00000000000000355, -82.50000000000001421 ) ) ;
#5520 = ORIENTED_EDGE ( 'NONE', *, *, #2125, .F. ) ;
#5521 = EDGE_CURVE ( 'NONE', #8998, #23, #5598, .T. ) ;
#5522 = DIRECTION ( 'NONE',  ( 0.7071067811865439090, 8.659560562354889717E-17, -0.7071067811865512365 ) ) ;
#5523 = DIRECTION ( 'NONE',  ( -0.000000000000000000, -0.000000000000000000, -1.000000000000000000 ) ) ;
#5524 = CARTESIAN_POINT ( 'NONE',  ( -1.750000000000013101, -1.749999999999997780, 0.000000000000000000 ) ) ;
#5525 = ORIENTED_EDGE ( 'NONE', *, *, #7044, .F. ) ;
#5526 = ORIENTED_EDGE ( 'NONE', *, *, #9026, .T. ) ;
#5527 = CONTEXT_DEPENDENT_SHAPE_REPRESENTATION ( #684, #2333 ) ;
#5528 = ADVANCED_FACE ( 'NONE', ( #4828 ), #7746, .F. ) ;
#5529 = VECTOR ( 'NONE', #8514, 999.9999999999998863 ) ;
#5530 = DIRECTION ( 'NONE',  ( -0.000000000000000000, -0.000000000000000000, -1.000000000000000000 ) ) ;
#5531 = DIRECTION ( 'NONE',  ( 0.000000000000000000, -0.7071067811865473507, -0.7071067811865477948 ) ) ;
#5532 = CARTESIAN_POINT ( 'NONE',  ( 4.000000000000000000, 14.14213562373247868, 12.58213562373372341 ) ) ;
#5533 = CARTESIAN_POINT ( 'NONE',  ( 0.000000000000000000, -34.00000000000001421, 32.00000000000000000 ) ) ;
#5534 = CARTESIAN_POINT ( 'NONE',  ( -27.28672223502583449, 5.374373886926214539, 0.8093214368023373684 ) ) ;
#5535 = VERTEX_POINT ( 'NONE', #7613 ) ;
#5536 = EDGE_CURVE ( 'NONE', #5896, #6890, #7880, .T. ) ;
#5537 = CARTESIAN_POINT ( 'NONE',  ( 25.50000000000000355, 3.673940397442056417E-16, 10.00000000000000000 ) ) ;
#5538 = AXIS2_PLACEMENT_3D ( 'NONE', #5992, #5938, #5218 ) ;
#5539 = VERTEX_POINT ( 'NONE', #6188 ) ;
#5540 = EDGE_CURVE ( 'NONE', #9435, #5792, #4678, .T. ) ;
#5541 = CARTESIAN_POINT ( 'NONE',  ( 0.000000000000000000, 0.000000000000000000, 50.00000000000000000 ) ) ;
#5542 = EDGE_CURVE ( 'NONE', #4079, #2481, #5250, .T. ) ;
#5543 = EDGE_CURVE ( 'NONE', #2498, #720, #2736, .T. ) ;
#5544 = DIRECTION ( 'NONE',  ( -1.000000000000000000, 0.000000000000000000, 0.000000000000000000 ) ) ;
#5545 = DIRECTION ( 'NONE',  ( -0.000000000000000000, 1.000000000000000000, -0.000000000000000000 ) ) ;
#5546 = CARTESIAN_POINT ( 'NONE',  ( 3.500000000000000444, -6.505213034913026604E-16, 1.500000000000000000 ) ) ;
#5547 = VECTOR ( 'NONE', #9279, 1000.000000000000000 ) ;
#5548 = LINE ( 'NONE', #7569, #724 ) ;
#5549 = VERTEX_POINT ( 'NONE', #1946 ) ;
#5550 = ORIENTED_EDGE ( 'NONE', *, *, #2557, .T. ) ;
#5551 = DIRECTION ( 'NONE',  ( -9.540979117872439019E-17, -0.9997175446104181740, 0.02376617340079498208 ) ) ;
#5552 = ORIENTED_EDGE ( 'NONE', *, *, #6254, .F. ) ;
#5553 = EDGE_CURVE ( 'NONE', #106, #2851, #8803, .T. ) ;
#5554 = FACE_BOUND ( 'NONE', #1289, .T. ) ;
#5555 = ADVANCED_FACE ( 'NONE', ( #318 ), #9097, .F. ) ;
#5556 = CARTESIAN_POINT ( 'NONE',  ( 60.00000000000000000, -30.00000000000000355, -82.50000000000001421 ) ) ;
#5557 = EDGE_CURVE ( 'NONE', #3651, #7789, #6215, .T. ) ;
#5558 = DIRECTION ( 'NONE',  ( 0.000000000000000000, 0.000000000000000000, 1.000000000000000000 ) ) ;
#5559 = CARTESIAN_POINT ( 'NONE',  ( 27.61161645726459568, 3.165483362335713480, 0.7903941804162394336 ) ) ;
#5560 = AXIS2_PLACEMENT_3D ( 'NONE', #4288, #4908, #5780 ) ;
#5561 = DIRECTION ( 'NONE',  ( -1.000000000000000000, 0.000000000000000000, 0.000000000000000000 ) ) ;
#5562 = ORIENTED_EDGE ( 'NONE', *, *, #474, .F. ) ;
#5563 = ORIENTED_EDGE ( 'NONE', *, *, #6593, .T. ) ;
#5564 =( BOUNDED_CURVE ( )  B_SPLINE_CURVE ( 3, ( #7657, #1843, #1071, #4007 ),
 .UNSPECIFIED., .F., .T. ) 
 B_SPLINE_CURVE_WITH_KNOTS ( ( 4, 4 ),
 ( 5.235987755982987935, 5.613918313269388172 ),
 .UNSPECIFIED. ) 
 CURVE ( )  GEOMETRIC_REPRESENTATION_ITEM ( )  RATIONAL_B_SPLINE_CURVE ( ( 1.000000000000000000, 0.9881327504826167285, 0.9881327504826167285, 1.000000000000000000 ) ) 
 REPRESENTATION_ITEM ( '' )  );
#5565 = CYLINDRICAL_SURFACE ( 'NONE', #7308, 7.250000000000002665 ) ;
#5566 = ORIENTED_EDGE ( 'NONE', *, *, #8162, .T. ) ;
#5567 = FACE_OUTER_BOUND ( 'NONE', #5883, .T. ) ;
#5568 = LINE ( 'NONE', #6815, #2441 ) ;
#5569 = ORIENTED_EDGE ( 'NONE', *, *, #1889, .F. ) ;
#5570 = AXIS2_PLACEMENT_3D ( 'NONE', #6640, #8889, #1541 ) ;
#5571 = CYLINDRICAL_SURFACE ( 'NONE', #8225, 11.00000000000000711 ) ;
#5572 = DIRECTION ( 'NONE',  ( -0.000000000000000000, -0.000000000000000000, -1.000000000000000000 ) ) ;
#5573 = VECTOR ( 'NONE', #581, 1000.000000000000000 ) ;
#5574 = DIRECTION ( 'NONE',  ( 0.000000000000000000, 0.000000000000000000, -1.000000000000000000 ) ) ;
#5575 = CARTESIAN_POINT ( 'NONE',  ( -26.21170834203230982, -53.97171801779368394, -2.612255525622733554 ) ) ;
#5576 = VERTEX_POINT ( 'NONE', #360 ) ;
#5577 = VERTEX_POINT ( 'NONE', #4785 ) ;
#5578 = AXIS2_PLACEMENT_3D ( 'NONE', #9001, #5409, #3867 ) ;
#5579 = CARTESIAN_POINT ( 'NONE',  ( 0.000000000000000000, 0.000000000000000000, 1.000000000000021760 ) ) ;
#5580 = DIRECTION ( 'NONE',  ( 0.000000000000000000, -1.000000000000000000, 0.000000000000000000 ) ) ;
#5581 = CARTESIAN_POINT ( 'NONE',  ( -27.00000000000000000, -43.00000000000000000, 11.99999999999999645 ) ) ;
#5582 = LINE ( 'NONE', #1149, #7019 ) ;
#5583 = AXIS2_PLACEMENT_3D ( 'NONE', #9145, #5608, #1995 ) ;
#5584 = ORIENTED_EDGE ( 'NONE', *, *, #3139, .T. ) ;
#5585 = EDGE_LOOP ( 'NONE', ( #8499, #8343, #5831, #1458 ) ) ;
#5586 = ORIENTED_EDGE ( 'NONE', *, *, #156, .F. ) ;
#5587 = DIRECTION ( 'NONE',  ( 0.000000000000000000, 0.000000000000000000, 1.000000000000000000 ) ) ;
#5588 = DIRECTION ( 'NONE',  ( -1.000000000000000000, 0.000000000000000000, 0.000000000000000000 ) ) ;
#5589 = AXIS2_PLACEMENT_3D ( 'NONE', #752, #6667, #5941 ) ;
#5590 = CARTESIAN_POINT ( 'NONE',  ( 5.000000000000000888, 0.000000000000000000, 0.000000000000000000 ) ) ;
#5591 = CARTESIAN_POINT ( 'NONE',  ( 5.000000000000000000, -18.47759065022790637, -6.903668647298391470 ) ) ;
#5592 = ADVANCED_FACE ( 'NONE', ( #7808 ), #4156, .T. ) ;
#5593 = CIRCLE ( 'NONE', #3287, 1.560000000000134168 ) ;
#5594 = PLANE ( 'NONE',  #1036 ) ;
#5595 = EDGE_CURVE ( 'NONE', #7535, #7179, #4111, .T. ) ;
#5596 = EDGE_LOOP ( 'NONE', ( #6759, #1823, #8740, #1085 ) ) ;
#5597 = ORIENTED_EDGE ( 'NONE', *, *, #7911, .T. ) ;
#5598 = CIRCLE ( 'NONE', #1917, 1.560000000002236709 ) ;
#5599 = ORIENTED_EDGE ( 'NONE', *, *, #1532, .T. ) ;
#5600 = FACE_BOUND ( 'NONE', #2420, .T. ) ;
#5601 = FACE_OUTER_BOUND ( 'NONE', #5752, .T. ) ;
#5602 = VECTOR ( 'NONE', #1421, 1000.000000000000000 ) ;
#5604 = EDGE_CURVE ( 'NONE', #4382, #1163, #9237, .T. ) ;
#5603 = DIRECTION ( 'NONE',  ( 0.000000000000000000, 0.000000000000000000, -1.000000000000000000 ) ) ;
#5605 = CIRCLE ( 'NONE', #3904, 0.7500000000000015543 ) ;
#5606 = CARTESIAN_POINT ( 'NONE',  ( 25.50000000000000355, 2.360423844116556880E-13, 15.00000000000000000 ) ) ;
#5607 =( REPRESENTATION_RELATIONSHIP ('NONE','NONE', #1933, #6964 ) REPRESENTATION_RELATIONSHIP_WITH_TRANSFORMATION ( #6879 )SHAPE_REPRESENTATION_RELATIONSHIP( ) );
#5608 = DIRECTION ( 'NONE',  ( 0.000000000000000000, 1.000000000000000000, 0.000000000000000000 ) ) ;
#5609 = VERTEX_POINT ( 'NONE', #3428 ) ;
#5610 = EDGE_LOOP ( 'NONE', ( #2871, #5919, #3368, #8444, #491, #8871, #8720, #6380 ) ) ;
#5611 = EDGE_CURVE ( 'NONE', #4522, #2905, #3571, .T. ) ;
#5612 = CARTESIAN_POINT ( 'NONE',  ( 0.000000000000000000, 9.603694566548697359E-13, 21.56000000000303984 ) ) ;
#5613 = EDGE_LOOP ( 'NONE', ( #5621, #4503, #4893, #6319 ) ) ;
#5614 = LINE ( 'NONE', #3347, #5043 ) ;
#5615 = CARTESIAN_POINT ( 'NONE',  ( 27.00000000000000000, 43.00000000000000000, 11.99999999999999645 ) ) ;
#5616 = DIRECTION ( 'NONE',  ( 1.000000000000000000, 0.000000000000000000, 0.000000000000000000 ) ) ;
#5617 = FACE_BOUND ( 'NONE', #479, .T. ) ;
#5618 =( BOUNDED_CURVE ( )  B_SPLINE_CURVE ( 3, ( #1548, #5978, #7406, #8181 ),
 .UNSPECIFIED., .F., .F. ) 
 B_SPLINE_CURVE_WITH_KNOTS ( ( 4, 4 ),
 ( 4.712388980384689674, 7.853981633974482790 ),
 .UNSPECIFIED. ) 
 CURVE ( )  GEOMETRIC_REPRESENTATION_ITEM ( )  RATIONAL_B_SPLINE_CURVE ( ( 1.000000000000000000, 0.3333333333333333703, 0.3333333333333333703, 1.000000000000000000 ) ) 
 REPRESENTATION_ITEM ( '' )  );
#5619 = CARTESIAN_POINT ( 'NONE',  ( -60.00000000000000000, 0.000000000000000000, 23.99999999999998579 ) ) ;
#5620 = DIRECTION ( 'NONE',  ( 1.000000000000000000, -0.000000000000000000, -0.000000000000000000 ) ) ;
#5621 = ORIENTED_EDGE ( 'NONE', *, *, #3128, .F. ) ;
#5622 = ORIENTED_EDGE ( 'NONE', *, *, #3712, .T. ) ;
#5623 = AXIS2_PLACEMENT_3D ( 'NONE', #6635, #1581, #765 ) ;
#5624 = DIRECTION ( 'NONE',  ( -0.000000000000000000, -0.000000000000000000, 1.000000000000000000 ) ) ;
#5625 = AXIS2_PLACEMENT_3D ( 'NONE', #7136, #557, #4309 ) ;
#5626 = CARTESIAN_POINT ( 'NONE',  ( 27.00000000000000355, 35.00000000000000000, 59.00000000000000000 ) ) ;
#5627 = CARTESIAN_POINT ( 'NONE',  ( -53.29490495164537833, 27.56180520566615044, -81.40266088840108694 ) ) ;
#5628 = EDGE_LOOP ( 'NONE', ( #9100, #8831, #2098, #4200 ) ) ;
#5629 = VERTEX_POINT ( 'NONE', #7951 ) ;
#5630 = ADVANCED_FACE ( 'NONE', ( #8761 ), #72, .T. ) ;
#5631 = ORIENTED_EDGE ( 'NONE', *, *, #8243, .F. ) ;
#5632 = AXIS2_PLACEMENT_3D ( 'NONE', #7168, #590, #1355 ) ;
#5633 = EDGE_LOOP ( 'NONE', ( #6322, #4926, #2009, #524 ) ) ;
#5634 = CIRCLE ( 'NONE', #5783, 0.7499999999986606269 ) ;
#5635 = CARTESIAN_POINT ( 'NONE',  ( 19.00000000000000000, 2.143131898507868248E-15, -17.50000000000000000 ) ) ;
#5636 = DIRECTION ( 'NONE',  ( -0.000000000000000000, -0.000000000000000000, -1.000000000000000000 ) ) ;
#5637 = EDGE_CURVE ( 'NONE', #2574, #4808, #1363, .T. ) ;
#5638 = CARTESIAN_POINT ( 'NONE',  ( 0.000000000000000000, 0.000000000000000000, 28.50000000000000355 ) ) ;
#5639 = CARTESIAN_POINT ( 'NONE',  ( -53.29490495164537833, -15.90990257669733943, -85.90990257669729147 ) ) ;
#5640 = CIRCLE ( 'NONE', #5489, 0.7500000000017874591 ) ;
#5641 = AXIS2_PLACEMENT_3D ( 'NONE', #8182, #7264, #2275 ) ;
#5642 = FACE_BOUND ( 'NONE', #4305, .T. ) ;
#5643 = CIRCLE ( 'NONE', #414, 18.49999999999998934 ) ;
#5644 = ORIENTED_EDGE ( 'NONE', *, *, #2137, .F. ) ;
#5645 = ORIENTED_EDGE ( 'NONE', *, *, #9181, .F. ) ;
#5646 = ORIENTED_EDGE ( 'NONE', *, *, #3834, .T. ) ;
#5647 = CIRCLE ( 'NONE', #6716, 26.99999999999999645 ) ;
#5648 = DIRECTION ( 'NONE',  ( 0.000000000000000000, 0.000000000000000000, -1.000000000000000000 ) ) ;
#5649 = VECTOR ( 'NONE', #4936, 999.9999999999998863 ) ;
#5650 = AXIS2_PLACEMENT_3D ( 'NONE', #444, #1156, #5544 ) ;
#5651 = CARTESIAN_POINT ( 'NONE',  ( 5.000000000000000000, 9.603694566548697359E-13, 20.00000000000290612 ) ) ;
#5652 = AXIS2_PLACEMENT_3D ( 'NONE', #3482, #2776, #7861 ) ;
#5653 = CARTESIAN_POINT ( 'NONE',  ( 3.499999999999999556, 0.000000000000000000, 0.000000000000000000 ) ) ;
#5654 = CARTESIAN_POINT ( 'NONE',  ( 2.499999999999998668, 3.367778697655220519E-16, 21.00000000000000000 ) ) ;
#5655 = PRODUCT_RELATED_PRODUCT_CATEGORY ( 'part', '', ( #7384 ) ) ;
#5656 = ORIENTED_EDGE ( 'NONE', *, *, #4026, .F. ) ;
#5657 = EDGE_CURVE ( 'NONE', #975, #3514, #7127, .T. ) ;
#5658 = ORIENTED_EDGE ( 'NONE', *, *, #4715, .F. ) ;
#5659 = CARTESIAN_POINT ( 'NONE',  ( -3.795548148769716690, 27.16282829747752103, 0.4246316111951826122 ) ) ;
#5660 = VERTEX_POINT ( 'NONE', #4919 ) ;
#5661 = EDGE_CURVE ( 'NONE', #450, #1766, #5758, .T. ) ;
#5662 = EDGE_CURVE ( 'NONE', #3407, #1534, #1282, .T. ) ;
#5663 = DIRECTION ( 'NONE',  ( -0.7071067811865470176, 0.000000000000000000, -0.7071067811865481278 ) ) ;
#5664 = AXIS2_PLACEMENT_3D ( 'NONE', #6382, #9291, #2729 ) ;
#5665 = CARTESIAN_POINT ( 'NONE',  ( 5.000000000000000000, 7.653668647300657213, -19.22759065022689384 ) ) ;
#5666 = EDGE_CURVE ( 'NONE', #2437, #8069, #7891, .T. ) ;
#5667 = PLANE ( 'NONE',  #4308 ) ;
#5668 = DIRECTION ( 'NONE',  ( -1.000000000000000000, 0.000000000000000000, 0.000000000000000000 ) ) ;
#5669 = VECTOR ( 'NONE', #7903, 1000.000000000000000 ) ;
#5670 = CARTESIAN_POINT ( 'NONE',  ( 26.79453276911118564, 6.186305604711932027, 0.4929139230000564864 ) ) ;
#5671 = EDGE_LOOP ( 'NONE', ( #637, #8350, #1602, #4022 ) ) ;
#5672 = VERTEX_POINT ( 'NONE', #4344 ) ;
#5673 = EDGE_CURVE ( 'NONE', #2622, #6180, #7897, .T. ) ;
#5674 = CONTEXT_DEPENDENT_SHAPE_REPRESENTATION ( #4247, #1234 ) ;
#5675 = EDGE_CURVE ( 'NONE', #5465, #4422, #6982, .T. ) ;
#5676 = ADVANCED_FACE ( 'NONE', ( #6560 ), #2082, .F. ) ;
#5677 = CARTESIAN_POINT ( 'NONE',  ( 0.000000000000000000, -35.00000000000000000, 32.00000000000000000 ) ) ;
#5679 = EDGE_CURVE ( 'NONE', #4271, #1738, #597, .T. ) ;
#5678 = DIRECTION ( 'NONE',  ( -1.000000000000000000, -0.000000000000000000, -0.000000000000000000 ) ) ;
#5680 = DIRECTION ( 'NONE',  ( -1.000000000000000000, 0.000000000000000000, -0.000000000000000000 ) ) ;
#5681 = DIRECTION ( 'NONE',  ( 1.000000000000000000, 0.000000000000000000, 0.000000000000000000 ) ) ;
#5682 = VERTEX_POINT ( 'NONE', #2809 ) ;
#5683 = VERTEX_POINT ( 'NONE', #7994 ) ;
#5684 = EDGE_LOOP ( 'NONE', ( #4605, #3050, #8085, #4608 ) ) ;
#5685 = ORIENTED_EDGE ( 'NONE', *, *, #8922, .T. ) ;
#5686 = DIRECTION ( 'NONE',  ( -1.000000000000000000, -0.000000000000000000, -0.000000000000000000 ) ) ;
#5687 = CARTESIAN_POINT ( 'NONE',  ( -2.749999999999995559, 0.7500000000000000000, 1.500000000000000000 ) ) ;
#5688 = DIRECTION ( 'NONE',  ( -0.000000000000000000, -0.000000000000000000, -1.000000000000000000 ) ) ;
#5689 = DIRECTION ( 'NONE',  ( -1.000000000000000000, 0.000000000000000000, 0.000000000000000000 ) ) ;
#5690 = FACE_BOUND ( 'NONE', #1712, .T. ) ;
#5691 = ORIENTED_EDGE ( 'NONE', *, *, #7963, .T. ) ;
#5692 = VERTEX_POINT ( 'NONE', #8038 ) ;
#5693 = DIRECTION ( 'NONE',  ( -0.02850404145984966262, -0.02375651666412747012, -0.9993113366396091379 ) ) ;
#5694 = VERTEX_POINT ( 'NONE', #7220 ) ;
#5695 = CARTESIAN_POINT ( 'NONE',  ( 0.000000000000000000, 0.000000000000000000, 11.00000000000000000 ) ) ;
#5696 = CARTESIAN_POINT ( 'NONE',  ( -27.81257783158192254, 2.818165554823761632, 0.9523463990989800010 ) ) ;
#5697 = EDGE_CURVE ( 'NONE', #9340, #5087, #7853, .T. ) ;
#5698 = VECTOR ( 'NONE', #983, 1000.000000000000000 ) ;
#5699 = CARTESIAN_POINT ( 'NONE',  ( 27.00000000000000355, -34.99999999999999289, 5.000000000000003553 ) ) ;
#5700 = DIRECTION ( 'NONE',  ( -1.000000000000000000, -0.000000000000000000, -0.000000000000000000 ) ) ;
#5701 = CARTESIAN_POINT ( 'NONE',  ( -26.99999999999998934, -34.99999999999999289, 64.00000000000000000 ) ) ;
#5702 = ORIENTED_EDGE ( 'NONE', *, *, #8390, .T. ) ;
#5703 = ORIENTED_EDGE ( 'NONE', *, *, #9233, .F. ) ;
#5704 = CARTESIAN_POINT ( 'NONE',  ( -1.691658612279394402, 28.27209108258186987, 1.319590333518658065 ) ) ;
#5705 = ORIENTED_EDGE ( 'NONE', *, *, #6878, .T. ) ;
#5706 = CARTESIAN_POINT ( 'NONE',  ( -60.00000000000000000, 30.00000000000000000, -13.00000000000000000 ) ) ;
#5707 = CARTESIAN_POINT ( 'NONE',  ( -6.000000000000000888, 0.000000000000000000, 1.000000000000000000 ) ) ;
#5708 = LINE ( 'NONE', #7229, #5151 ) ;
#5709 = VECTOR ( 'NONE', #4730, 1000.000000000000000 ) ;
#5710 = DIRECTION ( 'NONE',  ( -0.000000000000000000, -0.000000000000000000, 1.000000000000000000 ) ) ;
#5711 = EDGE_CURVE ( 'NONE', #9400, #4833, #7383, .T. ) ;
#5712 = DIRECTION ( 'NONE',  ( -0.000000000000000000, 1.000000000000000000, -0.000000000000000000 ) ) ;
#5713 = CARTESIAN_POINT ( 'NONE',  ( 6.000000000000000888, 22.50000000000000355, 5.000000000000000000 ) ) ;
#5714 = EDGE_CURVE ( 'NONE', #7012, #2635, #5018, .T. ) ;
#5715 = ORIENTED_EDGE ( 'NONE', *, *, #2371, .T. ) ;
#5716 = ORIENTED_EDGE ( 'NONE', *, *, #5595, .T. ) ;
#5717 = EDGE_CURVE ( 'NONE', #3765, #4223, #36, .T. ) ;
#5718 = EDGE_CURVE ( 'NONE', #5068, #7405, #2790, .T. ) ;
#5719 = AXIS2_PLACEMENT_3D ( 'NONE', #865, #1443, #2980 ) ;
#5720 = DIRECTION ( 'NONE',  ( 0.000000000000000000, 0.000000000000000000, -1.000000000000000000 ) ) ;
#5721 = ITEM_DEFINED_TRANSFORMATION ( 'NONE', 'NONE', #8678,  #1614 ) ;
#5722 = CYLINDRICAL_SURFACE ( 'NONE', #3484, 17.50000000000000000 ) ;
#5723 = CARTESIAN_POINT ( 'NONE',  ( 6.000000000000000888, -22.50000000000000355, 5.000000000000000000 ) ) ;
#5724 = CARTESIAN_POINT ( 'NONE',  ( 60.00000000000000000, -15.90990257669733943, -82.90990257669729147 ) ) ;
#5725 = ORIENTED_EDGE ( 'NONE', *, *, #8833, .F. ) ;
#5726 = EDGE_LOOP ( 'NONE', ( #5897, #9047, #166, #7763 ) ) ;
#5727 = CIRCLE ( 'NONE', #9084, 15.00000000000000000 ) ;
#5728 = ORIENTED_EDGE ( 'NONE', *, *, #9402, .F. ) ;
#5729 = ORIENTED_EDGE ( 'NONE', *, *, #4998, .T. ) ;
#5730 = EDGE_CURVE ( 'NONE', #3148, #5750, #3247, .T. ) ;
#5731 = CARTESIAN_POINT ( 'NONE',  ( -4.119968255444916849E-15, -3.500000000000000000, 1.500000000000000000 ) ) ;
#5732 =( REPRESENTATION_RELATIONSHIP ('NONE','NONE', #1933, #8501 ) REPRESENTATION_RELATIONSHIP_WITH_TRANSFORMATION ( #3544 )SHAPE_REPRESENTATION_RELATIONSHIP( ) );
#5733 = CARTESIAN_POINT ( 'NONE',  ( 5.000000000000000000, -20.00000000000120437, -1.559999999999665432 ) ) ;
#5734 = CARTESIAN_POINT ( 'NONE',  ( 41.99999999999999289, 12.50000000000000355, -100.0000000000000000 ) ) ;
#5735 = AXIS2_PLACEMENT_3D ( 'NONE', #7974, #3448, #4136 ) ;
#5736 = ADVANCED_FACE ( 'NONE', ( #4483 ), #3763, .F. ) ;
#5737 = DIRECTION ( 'NONE',  ( -0.000000000000000000, 1.000000000000000000, 0.000000000000000000 ) ) ;
#5738 = FACE_BOUND ( 'NONE', #4510, .T. ) ;
#5739 = AXIS2_PLACEMENT_3D ( 'NONE', #6240, #9106, #6152 ) ;
#5740 = VERTEX_POINT ( 'NONE', #928 ) ;
#5741 = DIRECTION ( 'NONE',  ( 0.000000000000000000, 0.000000000000000000, 1.000000000000000000 ) ) ;
#5742 = ORIENTED_EDGE ( 'NONE', *, *, #3413, .F. ) ;
#5743 = FACE_BOUND ( 'NONE', #4603, .T. ) ;
#5744 = VECTOR ( 'NONE', #1711, 1000.000000000000000 ) ;
#5745 = CYLINDRICAL_SURFACE ( 'NONE', #9461, 22.50000000000000000 ) ;
#5746 = DIRECTION ( 'NONE',  ( -1.000000000000000000, 0.000000000000000000, 0.000000000000000000 ) ) ;
#5747 = DIRECTION ( 'NONE',  ( 1.000000000000000000, 0.000000000000000000, 0.000000000000000000 ) ) ;
#5748 = CARTESIAN_POINT ( 'NONE',  ( 0.8594978869057854354, -28.44192451354556539, 1.454119780865607447 ) ) ;
#5749 = EDGE_LOOP ( 'NONE', ( #8832, #4588 ) ) ;
#5750 = VERTEX_POINT ( 'NONE', #8092 ) ;
#5751 = CARTESIAN_POINT ( 'NONE',  ( 5.000000000000000000, -18.47759065022790637, -8.403668647301127947 ) ) ;
#5752 = EDGE_LOOP ( 'NONE', ( #3816, #3766, #4212, #7359, #648, #2385, #6920, #817 ) ) ;
#5753 = EDGE_CURVE ( 'NONE', #694, #23, #5260, .T. ) ;
#5754 = DIRECTION ( 'NONE',  ( -1.000000000000000000, 0.000000000000000000, 0.000000000000000000 ) ) ;
#5755 = CIRCLE ( 'NONE', #6669, 3.000000000000002665 ) ;
#5756 = CARTESIAN_POINT ( 'NONE',  ( 0.000000000000000000, 22.50000000000000355, 2.000000000000013767 ) ) ;
#5757 = FACE_OUTER_BOUND ( 'NONE', #88, .T. ) ;
#5758 = CIRCLE ( 'NONE', #1603, 2.999999999999999112 ) ;
#5759 = DIRECTION ( 'NONE',  ( 0.000000000000000000, 1.000000000000000000, 0.000000000000000000 ) ) ;
#5760 = EDGE_CURVE ( 'NONE', #6515, #2884, #6854, .T. ) ;
#5761 = FACE_OUTER_BOUND ( 'NONE', #8285, .T. ) ;
#5762 = DIRECTION ( 'NONE',  ( 1.000000000000000000, 0.000000000000000000, 0.000000000000000000 ) ) ;
#5763 = EDGE_LOOP ( 'NONE', ( #5352, #7926 ) ) ;
#5764 = VERTEX_POINT ( 'NONE', #4444 ) ;
#5765 = LINE ( 'NONE', #1277, #4721 ) ;
#5766 = CARTESIAN_POINT ( 'NONE',  ( 3.000000000000000444, 3.673940397442060361E-16, 5.000000000000000000 ) ) ;
#5767 = CARTESIAN_POINT ( 'NONE',  ( 3.000000000000000000, 22.50000000000000355, 15.00000000000000000 ) ) ;
#5768 = DIRECTION ( 'NONE',  ( 0.000000000000000000, -1.000000000000000000, 0.000000000000000000 ) ) ;
#5769 = VERTEX_POINT ( 'NONE', #6080 ) ;
#5770 = ORIENTED_EDGE ( 'NONE', *, *, #8737, .T. ) ;
#5771 = ORIENTED_EDGE ( 'NONE', *, *, #5697, .T. ) ;
#5772 = EDGE_CURVE ( 'NONE', #6722, #4478, #3046, .T. ) ;
#5773 = ORIENTED_EDGE ( 'NONE', *, *, #7109, .T. ) ;
#5774 = EDGE_CURVE ( 'NONE', #1969, #9413, #6173, .T. ) ;
#5775 = DIRECTION ( 'NONE',  ( -1.000000000000000000, -0.000000000000000000, -0.000000000000000000 ) ) ;
#5776 = CARTESIAN_POINT ( 'NONE',  ( 0.000000000000000000, 22.50000000000000355, 2.000000000000013767 ) ) ;
#5777 = VECTOR ( 'NONE', #8835, 1000.000000000000114 ) ;
#5778 = CARTESIAN_POINT ( 'NONE',  ( 5.000000000000000000, -18.47759065022790637, -7.653668647299759265 ) ) ;
#5779 = PRODUCT_DEFINITION_SHAPE ( 'NONE', 'NONE',  #9481 ) ;
#5780 = DIRECTION ( 'NONE',  ( 0.000000000000000000, 0.000000000000000000, 1.000000000000000000 ) ) ;
#5781 = CARTESIAN_POINT ( 'NONE',  ( 0.000000000000000000, -29.99999999999999289, 64.00000000000000000 ) ) ;
#5782 = ORIENTED_EDGE ( 'NONE', *, *, #8369, .T. ) ;
#5783 = AXIS2_PLACEMENT_3D ( 'NONE', #2230, #2954, #5166 ) ;
#5784 = CARTESIAN_POINT ( 'NONE',  ( 0.000000000000000000, 0.000000000000000000, 50.00000000000000000 ) ) ;
#5785 = ORIENTED_EDGE ( 'NONE', *, *, #6131, .F. ) ;
#5786 = CARTESIAN_POINT ( 'NONE',  ( 5.000000000000000000, 18.47759065022658120, 7.653668647302884764 ) ) ;
#5787 = CYLINDRICAL_SURFACE ( 'NONE', #8758, 6.000000000000001776 ) ;
#5788 = AXIS2_PLACEMENT_3D ( 'NONE', #5786, #8713, #2131 ) ;
#5789 = DIRECTION ( 'NONE',  ( 1.000000000000000000, -0.000000000000000000, -0.000000000000000000 ) ) ;
#5790 = AXIS2_PLACEMENT_3D ( 'NONE', #2215, #5147, #8841 ) ;
#5791 = CARTESIAN_POINT ( 'NONE',  ( -2.813989238837524276, -27.81487630015522328, 0.9541967664096193680 ) ) ;
#5792 = VERTEX_POINT ( 'NONE', #8992 ) ;
#5793 = ORIENTED_EDGE ( 'NONE', *, *, #5440, .T. ) ;
#5794 = VECTOR ( 'NONE', #3831, 1000.000000000000000 ) ;
#5795 = ORIENTED_EDGE ( 'NONE', *, *, #9399, .T. ) ;
#5796 = AXIS2_PLACEMENT_3D ( 'NONE', #4469, #2314, #8170 ) ;
#5797 = CARTESIAN_POINT ( 'NONE',  ( 0.000000000000000000, -7.653668647301985040, 18.47759065022880520 ) ) ;
#5798 = DIRECTION ( 'NONE',  ( -1.000000000000000000, 0.000000000000000000, 0.000000000000000000 ) ) ;
#5799 = DIRECTION ( 'NONE',  ( -0.000000000000000000, -0.000000000000000000, 1.000000000000000000 ) ) ;
#5800 = DIRECTION ( 'NONE',  ( -1.000000000000000000, 0.000000000000000000, 0.000000000000000000 ) ) ;
#5801 = AXIS2_PLACEMENT_3D ( 'NONE', #2546, #3990, #6779 ) ;
#5802 = DIRECTION ( 'NONE',  ( 0.000000000000000000, 0.000000000000000000, 1.000000000000000000 ) ) ;
#5803 = DIRECTION ( 'NONE',  ( -1.000000000000000000, 0.000000000000000000, 0.000000000000000000 ) ) ;
#5804 = VERTEX_POINT ( 'NONE', #6797 ) ;
#5805 = ORIENTED_EDGE ( 'NONE', *, *, #8006, .T. ) ;
#5806 = FACE_OUTER_BOUND ( 'NONE', #4971, .T. ) ;
#5807 = CONTEXT_DEPENDENT_SHAPE_REPRESENTATION ( #5426, #29 ) ;
#5808 = AXIS2_PLACEMENT_3D ( 'NONE', #3098, #6037, #2386 ) ;
#5809 = CIRCLE ( 'NONE', #5216, 60.00000000000000000 ) ;
#5810 = DIRECTION ( 'NONE',  ( -0.000000000000000000, -0.000000000000000000, -1.000000000000000000 ) ) ;
#5811 = DIRECTION ( 'NONE',  ( 1.000000000000000000, 0.000000000000000000, 0.000000000000000000 ) ) ;
#5812 = VERTEX_POINT ( 'NONE', #118 ) ;
#5813 = ORIENTED_EDGE ( 'NONE', *, *, #2127, .F. ) ;
#5814 = EDGE_CURVE ( 'NONE', #8237, #523, #8898, .T. ) ;
#5815 = ORIENTED_EDGE ( 'NONE', *, *, #8365, .T. ) ;
#5816 = VECTOR ( 'NONE', #7644, 1000.000000000000000 ) ;
#5817 = EDGE_LOOP ( 'NONE', ( #4171, #1746, #8317, #6376 ) ) ;
#5818 = DIRECTION ( 'NONE',  ( 0.000000000000000000, 0.000000000000000000, -1.000000000000000000 ) ) ;
#5819 = CARTESIAN_POINT ( 'NONE',  ( -27.00000000000000000, 43.00000000000000000, 11.99999999999999645 ) ) ;
#5820 = FACE_OUTER_BOUND ( 'NONE', #618, .T. ) ;
#5821 = DIRECTION ( 'NONE',  ( 0.000000000000000000, 0.000000000000000000, 1.000000000000000000 ) ) ;
#5822 = B_SPLINE_CURVE_WITH_KNOTS ( 'NONE', 3,
 ( #9437, #3578, #6516, #4351, #2863, #8724, #2141, #695, #3627, #3605, #7609, #5408 ),
 .UNSPECIFIED., .F., .F.,
 ( 4, 2, 2, 2, 2, 4 ),
 ( 9.098896311893213187E-19, 0.001279392565614375721, 0.002558785131228750575, 0.003838177696843125212, 0.004477873979650310796, 0.005117570262457497680 ),
 .UNSPECIFIED. ) ;
#5823 = CYLINDRICAL_SURFACE ( 'NONE', #7049, 17.50000000000000355 ) ;
#5824 = EDGE_CURVE ( 'NONE', #4881, #1684, #7411, .T. ) ;
#5825 = FACE_BOUND ( 'NONE', #8621, .T. ) ;
#5826 = ORIENTED_EDGE ( 'NONE', *, *, #6627, .F. ) ;
#5827 = ADVANCED_FACE ( 'NONE', ( #5927 ), #8854, .F. ) ;
#5828 = FACE_OUTER_BOUND ( 'NONE', #2097, .T. ) ;
#5829 = ADVANCED_FACE ( 'NONE', ( #826 ), #8468, .F. ) ;
#5830 = EDGE_CURVE ( 'NONE', #6890, #6515, #4631, .T. ) ;
#5831 = ORIENTED_EDGE ( 'NONE', *, *, #6846, .F. ) ;
#5832 = PLANE ( 'NONE',  #350 ) ;
#5833 = CARTESIAN_POINT ( 'NONE',  ( 0.000000000000000000, 0.000000000000000000, 63.00000000000002842 ) ) ;
#5834 = CARTESIAN_POINT ( 'NONE',  ( 53.29490495164537833, -15.90990257669733943, -82.90990257669729147 ) ) ;
#5835 = DIRECTION ( 'NONE',  ( 0.000000000000000000, 0.000000000000000000, 1.000000000000000000 ) ) ;
#5836 = DIRECTION ( 'NONE',  ( 0.000000000000000000, 1.000000000000000000, 0.000000000000000000 ) ) ;
#5837 = ORIENTED_EDGE ( 'NONE', *, *, #1428, .T. ) ;
#5838 = VERTEX_POINT ( 'NONE', #880 ) ;
#5839 = ORIENTED_EDGE ( 'NONE', *, *, #6006, .T. ) ;
#5840 = ADVANCED_FACE ( 'NONE', ( #8281 ), #4387, .F. ) ;
#5841 = DIRECTION ( 'NONE',  ( 1.000000000000000000, 0.000000000000000000, 0.000000000000000000 ) ) ;
#5842 = CARTESIAN_POINT ( 'NONE',  ( -22.50000000000000000, -7.855833012397050680E-14, 5.000000000000000000 ) ) ;
#5843 = CIRCLE ( 'NONE', #1383, 0.7500000000000015543 ) ;
#5844 = EDGE_CURVE ( 'NONE', #4499, #3178, #1722, .T. ) ;
#5845 = FACE_OUTER_BOUND ( 'NONE', #1592, .T. ) ;
#5846 = DIRECTION ( 'NONE',  ( 0.000000000000000000, 0.000000000000000000, 1.000000000000000000 ) ) ;
#5847 = DIRECTION ( 'NONE',  ( 1.000000000000000000, 0.000000000000000000, 0.000000000000000000 ) ) ;
#5848 = DIRECTION ( 'NONE',  ( 1.000000000000000000, 0.000000000000000000, 0.000000000000000000 ) ) ;
#5849 = CIRCLE ( 'NONE', #7073, 2.999999999999999112 ) ;
#5850 = DIRECTION ( 'NONE',  ( -1.000000000000000000, 0.000000000000000000, 0.000000000000000000 ) ) ;
#5851 = ORIENTED_EDGE ( 'NONE', *, *, #8363, .T. ) ;
#5852 = ORIENTED_EDGE ( 'NONE', *, *, #1335, .T. ) ;
#5853 = DIRECTION ( 'NONE',  ( -1.000000000000000000, -0.000000000000000000, -0.000000000000000000 ) ) ;
#5854 = CARTESIAN_POINT ( 'NONE',  ( -22.50000000000000355, 0.000000000000000000, 2.000000000000039080 ) ) ;
#5855 = PRODUCT ( '3-Flange Yoke', '3-Flange Yoke', '', ( #1056 ) ) ;
#5856 = CARTESIAN_POINT ( 'NONE',  ( 30.00000000000000000, 3.673940397442059178E-15, 3.000000000000052847 ) ) ;
#5857 = CYLINDRICAL_SURFACE ( 'NONE', #2975, 2.999999999999999112 ) ;
#5858 = DIRECTION ( 'NONE',  ( 1.000000000000000000, 0.000000000000000000, 0.000000000000000000 ) ) ;
#5859 = VERTEX_POINT ( 'NONE', #8951 ) ;
#5860 = ORIENTED_EDGE ( 'NONE', *, *, #2807, .F. ) ;
#5861 = ORIENTED_EDGE ( 'NONE', *, *, #7954, .F. ) ;
#5862 = DIRECTION ( 'NONE',  ( -0.9998359049375277197, -0.0004305307730384466637, -0.01811015850312751307 ) ) ;
#5863 =( BOUNDED_CURVE ( )  B_SPLINE_CURVE ( 3, ( #2868, #8007, #7279, #2292 ),
 .UNSPECIFIED., .F., .T. ) 
 B_SPLINE_CURVE_WITH_KNOTS ( ( 4, 4 ),
 ( 2.356194490192345281, 3.926990816987240951 ),
 .UNSPECIFIED. ) 
 CURVE ( )  GEOMETRIC_REPRESENTATION_ITEM ( )  RATIONAL_B_SPLINE_CURVE ( ( 1.000000000000000000, 0.8047378541243652705, 0.8047378541243652705, 1.000000000000000000 ) ) 
 REPRESENTATION_ITEM ( '' )  );
#5864 = ORIENTED_EDGE ( 'NONE', *, *, #2137, .T. ) ;
#5865 = EDGE_CURVE ( 'NONE', #4910, #1656, #8311, .T. ) ;
#5866 = CARTESIAN_POINT ( 'NONE',  ( 0.000000000000000000, 22.50000000000000355, 5.000000000000000000 ) ) ;
#5867 = CARTESIAN_POINT ( 'NONE',  ( 32.00000000000000711, 29.99999999999997158, 0.000000000000000000 ) ) ;
#5868 = CARTESIAN_POINT ( 'NONE',  ( 2.000000000000000000, 0.000000000000000000, 13.66147716702868031 ) ) ;
#5869 = CYLINDRICAL_SURFACE ( 'NONE', #3255, 6.000000000000001776 ) ;
#5870 = AXIS2_PLACEMENT_3D ( 'NONE', #3136, #7598, #4627 ) ;
#5871 = DIRECTION ( 'NONE',  ( -1.000000000000000000, -0.000000000000000000, -0.000000000000000000 ) ) ;
#5872 = CARTESIAN_POINT ( 'NONE',  ( 0.000000000000000000, -34.99999999999999289, 32.00000000000000000 ) ) ;
#5873 = EDGE_LOOP ( 'NONE', ( #7085, #1659, #6910, #4373 ) ) ;
#5874 = CARTESIAN_POINT ( 'NONE',  ( -4.333301281932591564, -26.65000000000000213, 0.000000000000000000 ) ) ;
#5875 = ORIENTED_EDGE ( 'NONE', *, *, #6627, .T. ) ;
#5876 = DIRECTION ( 'NONE',  ( 0.000000000000000000, 0.000000000000000000, -1.000000000000000000 ) ) ;
#5877 = AXIS2_PLACEMENT_3D ( 'NONE', #9137, #6038, #315 ) ;
#5878 = CYLINDRICAL_SURFACE ( 'NONE', #5334, 1.559999999998939346 ) ;
#5879 = B_SPLINE_CURVE_WITH_KNOTS ( 'NONE', 3,
 ( #799, #8115, #851, #4559, #6727, #2247, #2354, #6626, #6819, #3738, #5902, #4462, #5180, #8261, #6053, #1575, #1624, #5229, #1723, #8163, #6675, #5384, #7482, #8826, #90, #4504 ),
 .UNSPECIFIED., .F., .F.,
 ( 4, 2, 2, 2, 2, 2, 2, 2, 2, 2, 2, 2, 4 ),
 ( 1.812491582141323212E-18, 0.002002306497011713607, 0.004004612994023425479, 0.005005766242529281415, 0.006006919491035139086, 0.007008072739540995022, 0.008009225988046852693, 0.01001153248505856456, 0.01101268573356442224, 0.01201383898207027817, 0.01301499223057613411, 0.01401614547908198831, 0.01601845197609370539 ),
 .UNSPECIFIED. ) ;
#5880 = FACE_OUTER_BOUND ( 'NONE', #4280, .T. ) ;
#5881 = EDGE_CURVE ( 'NONE', #4256, #5932, #3337, .T. ) ;
#5882 = DIRECTION ( 'NONE',  ( -1.000000000000000000, 0.000000000000000000, 0.000000000000000000 ) ) ;
#5883 = EDGE_LOOP ( 'NONE', ( #5178, #2170, #3420, #8963 ) ) ;
#5884 = CIRCLE ( 'NONE', #8948, 6.000000000000001776 ) ;
#5885 = ORIENTED_EDGE ( 'NONE', *, *, #4938, .T. ) ;
#5886 =( NAMED_UNIT ( * ) SI_UNIT ( $, .STERADIAN. ) SOLID_ANGLE_UNIT ( ) );
#5887 = ORIENTED_EDGE ( 'NONE', *, *, #3002, .F. ) ;
#5888 = LINE ( 'NONE', #5934, #1057 ) ;
#5889 = CARTESIAN_POINT ( 'NONE',  ( -26.99999999999998934, 32.49999999999998579, 61.50000000000000000 ) ) ;
#5890 = EDGE_CURVE ( 'NONE', #7651, #933, #8004, .T. ) ;
#5891 = LINE ( 'NONE', #5936, #4397 ) ;
#5892 = DIRECTION ( 'NONE',  ( 0.7071067811865456854, 0.000000000000000000, 0.7071067811865493491 ) ) ;
#5893 = CARTESIAN_POINT ( 'NONE',  ( -37.00000000000000711, -3.673940397442057600E-15, -70.00000000000000000 ) ) ;
#5894 = CYLINDRICAL_SURFACE ( 'NONE', #7123, 60.00000000000000000 ) ;
#5895 = DIRECTION ( 'NONE',  ( 0.000000000000000000, 0.000000000000000000, 1.000000000000000000 ) ) ;
#5896 = VERTEX_POINT ( 'NONE', #3280 ) ;
#5897 = ORIENTED_EDGE ( 'NONE', *, *, #1535, .F. ) ;
#5898 = DIRECTION ( 'NONE',  ( 0.000000000000000000, 0.000000000000000000, -1.000000000000000000 ) ) ;
#5899 = DIRECTION ( 'NONE',  ( -1.000000000000000000, -0.000000000000000000, -0.000000000000000000 ) ) ;
#5900 = VECTOR ( 'NONE', #3977, 1000.000000000000000 ) ;
#5901 = ORIENTED_EDGE ( 'NONE', *, *, #1430, .F. ) ;
#5902 = CARTESIAN_POINT ( 'NONE',  ( -1.356121383298963590, 28.66577847273270763, 1.695857589613878558 ) ) ;
#5903 = AXIS2_PLACEMENT_3D ( 'NONE', #3683, #5802, #4401 ) ;
#5904 = CONICAL_SURFACE ( 'NONE', #7896, 59.00000000000000000, 0.7853981633974415066 ) ;
#5905 = DIRECTION ( 'NONE',  ( -0.7071067811865439090, 0.000000000000000000, -0.7071067811865512365 ) ) ;
#5906 = CARTESIAN_POINT ( 'NONE',  ( 5.000000000000000000, 7.653668647300657213, -18.47759065022568237 ) ) ;
#5907 = ORIENTED_EDGE ( 'NONE', *, *, #7403, .T. ) ;
#5908 = VERTEX_POINT ( 'NONE', #3964 ) ;
#5909 = VECTOR ( 'NONE', #4119, 1000.000000000000000 ) ;
#5910 = ORIENTED_EDGE ( 'NONE', *, *, #6963, .F. ) ;
#5911 = DIRECTION ( 'NONE',  ( 0.000000000000000000, 1.000000000000000000, 0.000000000000000000 ) ) ;
#5912 = DIRECTION ( 'NONE',  ( -0.000000000000000000, -0.000000000000000000, -1.000000000000000000 ) ) ;
#5913 = LINE ( 'NONE', #2265, #8445 ) ;
#5914 = FACE_OUTER_BOUND ( 'NONE', #2862, .T. ) ;
#5915 = CARTESIAN_POINT ( 'NONE',  ( -31.99999999999999289, 0.000000000000000000, 32.00000000000000000 ) ) ;
#5916 = ADVANCED_FACE ( 'NONE', ( #6894 ), #4173, .F. ) ;
#5917 = CYLINDRICAL_SURFACE ( 'NONE', #1960, 11.00000000000000711 ) ;
#5918 =( BOUNDED_CURVE ( )  B_SPLINE_CURVE ( 3, ( #1479, #8829, #8882, #8016 ),
 .UNSPECIFIED., .F., .T. ) 
 B_SPLINE_CURVE_WITH_KNOTS ( ( 4, 4 ),
 ( 5.805906910357376383, 6.283185307179586232 ),
 .UNSPECIFIED. ) 
 CURVE ( )  GEOMETRIC_REPRESENTATION_ITEM ( )  RATIONAL_B_SPLINE_CURVE ( ( 1.000000000000000000, 0.9811070276743185659, 0.9811070276743185659, 1.000000000000000000 ) ) 
 REPRESENTATION_ITEM ( '' )  );
#5919 = ORIENTED_EDGE ( 'NONE', *, *, #907, .F. ) ;
#5920 = DIRECTION ( 'NONE',  ( 0.000000000000000000, 0.000000000000000000, 1.000000000000000000 ) ) ;
#5921 = VERTEX_POINT ( 'NONE', #9086 ) ;
#5922 = CIRCLE ( 'NONE', #9282, 30.00000000000000000 ) ;
#5923 = DIRECTION ( 'NONE',  ( -1.000000000000000000, -0.000000000000000000, -0.000000000000000000 ) ) ;
#5924 = EDGE_CURVE ( 'NONE', #4838, #4159, #4814, .T. ) ;
#5925 = DIRECTION ( 'NONE',  ( -0.000000000000000000, -0.000000000000000000, -1.000000000000000000 ) ) ;
#5926 = CARTESIAN_POINT ( 'NONE',  ( 4.000000000000000000, -14.14213562373112154, 12.58213562373271621 ) ) ;
#5927 = FACE_OUTER_BOUND ( 'NONE', #1545, .T. ) ;
#5928 = CIRCLE ( 'NONE', #7919, 7.250000000000002665 ) ;
#5929 = PRODUCT_DEFINITION_SHAPE ( 'NONE', 'NONE',  #3358 ) ;
#5930 = VERTEX_POINT ( 'NONE', #7557 ) ;
#5931 = ORIENTED_EDGE ( 'NONE', *, *, #608, .F. ) ;
#5932 = VERTEX_POINT ( 'NONE', #2477 ) ;
#5933 = ADVANCED_FACE ( 'NONE', ( #3189 ), #2519, .F. ) ;
#5934 = CARTESIAN_POINT ( 'NONE',  ( 60.00000000000000000, -15.90990257669733943, -51.09009742330271564 ) ) ;
#5935 = CARTESIAN_POINT ( 'NONE',  ( -12.37436867076458036, 12.37436867076458036, 19.62563132923542142 ) ) ;
#5936 = CARTESIAN_POINT ( 'NONE',  ( 53.29490495164537833, 27.56180520566615044, -134.0000000000000284 ) ) ;
#5937 = CIRCLE ( 'NONE', #8393, 17.50000000000000355 ) ;
#5938 = DIRECTION ( 'NONE',  ( -1.000000000000000000, 0.000000000000000000, 0.000000000000000000 ) ) ;
#5939 = FACE_OUTER_BOUND ( 'NONE', #197, .T. ) ;
#5940 = DIRECTION ( 'NONE',  ( 0.000000000000000000, 0.000000000000000000, -1.000000000000000000 ) ) ;
#5941 = DIRECTION ( 'NONE',  ( -0.7071067811865494601, 0.000000000000000000, 0.7071067811865454633 ) ) ;
#5942 = EDGE_CURVE ( 'NONE', #4405, #1500, #8323, .T. ) ;
#5943 = CIRCLE ( 'NONE', #5796, 30.00000000000000000 ) ;
#5944 = VERTEX_POINT ( 'NONE', #1698 ) ;
#5945 = EDGE_CURVE ( 'NONE', #3385, #7541, #7030, .T. ) ;
#5946 = VERTEX_POINT ( 'NONE', #261 ) ;
#5947 = CIRCLE ( 'NONE', #6261, 22.00000000000000355 ) ;
#5948 = EDGE_CURVE ( 'NONE', #2323, #4692, #4053, .T. ) ;
#5949 = ADVANCED_FACE ( 'NONE', ( #1113 ), #7602, .F. ) ;
#5950 = ORIENTED_EDGE ( 'NONE', *, *, #1889, .T. ) ;
#5951 = AXIS2_PLACEMENT_3D ( 'NONE', #3540, #8154, #8008 ) ;
#5952 = LINE ( 'NONE', #7432, #8258 ) ;
#5953 = CIRCLE ( 'NONE', #1807, 3.000000000000002665 ) ;
#5954 = AXIS2_PLACEMENT_3D ( 'NONE', #370, #993, #7725 ) ;
#5955 = FACE_OUTER_BOUND ( 'NONE', #121, .T. ) ;
#5956 = UNCERTAINTY_MEASURE_WITH_UNIT (LENGTH_MEASURE( 1.000000000000000082E-05 ), #1747, 'distance_accuracy_value', 'NONE');
#5957 = DIRECTION ( 'NONE',  ( -0.000000000000000000, -0.000000000000000000, -1.000000000000000000 ) ) ;
#5958 = VERTEX_POINT ( 'NONE', #5546 ) ;
#5959 = ORIENTED_EDGE ( 'NONE', *, *, #1663, .F. ) ;
#5960 = EDGE_CURVE ( 'NONE', #5995, #3553, #5500, .T. ) ;
#5961 = APPLICATION_PROTOCOL_DEFINITION ( 'draft international standard', 'automotive_design', 1998, #499 ) ;
#5962 = EDGE_CURVE ( 'NONE', #7596, #580, #1788, .T. ) ;
#5963 = CARTESIAN_POINT ( 'NONE',  ( 28.50000000000000355, 2.364097880450372804E-13, 1.500000000000041078 ) ) ;
#5964 = AXIS2_PLACEMENT_3D ( 'NONE', #1118, #8437, #8382 ) ;
#5965 = CIRCLE ( 'NONE', #6582, 3.000000000000000444 ) ;
#5966 = EDGE_CURVE ( 'NONE', #7881, #3433, #1886, .T. ) ;
#5967 = CARTESIAN_POINT ( 'NONE',  ( 52.42476942962458963, 29.19763577280652811, -80.99738777760514097 ) ) ;
#5968 = AXIS2_PLACEMENT_3D ( 'NONE', #8653, #6404, #4145 ) ;
#5969 = DIRECTION ( 'NONE',  ( 1.000000000000000000, 0.000000000000000000, 0.000000000000000000 ) ) ;
#5970 = CARTESIAN_POINT ( 'NONE',  ( 4.000000000000000000, 9.603694566548697359E-13, 20.00000000000290612 ) ) ;
#5971 = CARTESIAN_POINT ( 'NONE',  ( 5.000000000000000000, 18.47759065022580316, -6.903668647301629768 ) ) ;
#5972 = CARTESIAN_POINT ( 'NONE',  ( 4.000000000000000000, -14.14213562373248401, -14.14213562372942157 ) ) ;
#5973 = AXIS2_PLACEMENT_3D ( 'NONE', #2728, #6381, #7959 ) ;
#5974 = VERTEX_POINT ( 'NONE', #2664 ) ;
#5975 = AXIS2_PLACEMENT_3D ( 'NONE', #4773, #2425, #3906 ) ;
#5976 =( NAMED_UNIT ( * ) SI_UNIT ( $, .STERADIAN. ) SOLID_ANGLE_UNIT ( ) );
#5977 = ORIENTED_EDGE ( 'NONE', *, *, #4066, .T. ) ;
#5978 = CARTESIAN_POINT ( 'NONE',  ( 15.99999999999999822, -21.00000000000000000, -16.89999999999999858 ) ) ;
#5979 = CARTESIAN_POINT ( 'NONE',  ( -60.00000000000000000, 0.000000000000000000, 25.00000000000000000 ) ) ;
#5980 = LINE ( 'NONE', #2377, #6132 ) ;
#5981 =( BOUNDED_CURVE ( )  B_SPLINE_CURVE ( 3, ( #6217, #3961, #2567, #9042 ),
 .UNSPECIFIED., .F., .T. ) 
 B_SPLINE_CURVE_WITH_KNOTS ( ( 4, 4 ),
 ( 3.141592653589793116, 3.926990816987241395 ),
 .UNSPECIFIED. ) 
 CURVE ( )  GEOMETRIC_REPRESENTATION_ITEM ( )  RATIONAL_B_SPLINE_CURVE ( ( 1.000000000000000000, 0.9492530216741911220, 0.9492530216741911220, 1.000000000000000000 ) ) 
 REPRESENTATION_ITEM ( '' )  );
#5982 = DIRECTION ( 'NONE',  ( 0.000000000000000000, 0.000000000000000000, 1.000000000000000000 ) ) ;
#5983 = ORIENTED_EDGE ( 'NONE', *, *, #8544, .T. ) ;
#5984 = ORIENTED_EDGE ( 'NONE', *, *, #549, .T. ) ;
#5985 = EDGE_LOOP ( 'NONE', ( #5377, #8423, #1470, #3009, #4115, #6563, #4820 ) ) ;
#5986 = ORIENTED_EDGE ( 'NONE', *, *, #8833, .T. ) ;
#5987 = CARTESIAN_POINT ( 'NONE',  ( 27.00000000000000000, 43.00000000000000000, 11.99999999999999645 ) ) ;
#5988 = DIRECTION ( 'NONE',  ( 0.000000000000000000, 0.000000000000000000, 1.000000000000000000 ) ) ;
#5989 = AXIS2_PLACEMENT_3D ( 'NONE', #2704, #7209, #8561 ) ;
#5990 = EDGE_CURVE ( 'NONE', #3178, #4404, #6630, .T. ) ;
#5991 = CARTESIAN_POINT ( 'NONE',  ( 4.000000000000000000, -14.14213562373112154, 14.14213562373418220 ) ) ;
#5992 = CARTESIAN_POINT ( 'NONE',  ( -53.29490495164537833, -30.00000000000000000, -41.61356529332876875 ) ) ;
#5993 = CARTESIAN_POINT ( 'NONE',  ( 12.37436867076458036, 12.37436867076458036, 44.37436867076458213 ) ) ;
#5994 = CARTESIAN_POINT ( 'NONE',  ( 28.11123945536280644, -3.602653646940633614, 1.339368221304666262 ) ) ;
#5995 = VERTEX_POINT ( 'NONE', #4682 ) ;
#5996 = EDGE_LOOP ( 'NONE', ( #312, #8506 ) ) ;
#5997 = VECTOR ( 'NONE', #6384, 1000.000000000000000 ) ;
#5998 = CARTESIAN_POINT ( 'NONE',  ( -20.14434505884620918, -53.53579249963524234, -2.801156583491396734 ) ) ;
#5999 = DIRECTION ( 'NONE',  ( -1.000000000000000000, 0.000000000000000000, 0.000000000000000000 ) ) ;
#6000 = EDGE_LOOP ( 'NONE', ( #4895, #2698, #8557, #4315 ) ) ;
#6001 = DIRECTION ( 'NONE',  ( -0.5773502691896293948, -0.000000000000000000, -0.8164965809277234809 ) ) ;
#6002 = EDGE_CURVE ( 'NONE', #4498, #2113, #6129, .T. ) ;
#6003 = AXIS2_PLACEMENT_3D ( 'NONE', #5411, #8483, #8333 ) ;
#6004 = EDGE_CURVE ( 'NONE', #3384, #1832, #5564, .T. ) ;
#6005 = CARTESIAN_POINT ( 'NONE',  ( -0.7500000000000000000, -0.7500000000000000000, 0.000000000000000000 ) ) ;
#6006 = EDGE_CURVE ( 'NONE', #2331, #8797, #6937, .T. ) ;
#6007 = EDGE_CURVE ( 'NONE', #4903, #2056, #1093, .T. ) ;
#6008 = FACE_OUTER_BOUND ( 'NONE', #8682, .T. ) ;
#6009 = VERTEX_POINT ( 'NONE', #7843 ) ;
#6010 = ORIENTED_EDGE ( 'NONE', *, *, #1190, .F. ) ;
#6011 = APPLICATION_PROTOCOL_DEFINITION ( 'draft international standard', 'automotive_design', 1998, #1981 ) ;
#6012 = CARTESIAN_POINT ( 'NONE',  ( -53.29490495164537833, -3.673940397442057600E-15, -55.00000000000000711 ) ) ;
#6013 = DIRECTION ( 'NONE',  ( 0.000000000000000000, -0.7071067811865473507, -0.7071067811865477948 ) ) ;
#6014 = AXIS2_PLACEMENT_3D ( 'NONE', #5056, #3461, #4188 ) ;
#6015 = CARTESIAN_POINT ( 'NONE',  ( -30.99999999999996803, 0.000000000000000000, 32.00000000000000000 ) ) ;
#6016 = PRODUCT_DEFINITION_SHAPE ( 'NONE', 'NONE',  #9494 ) ;
#6017 = LINE ( 'NONE', #3799, #7390 ) ;
#6018 = DIRECTION ( 'NONE',  ( -0.7071067811865439090, 0.000000000000000000, -0.7071067811865511255 ) ) ;
#6019 = CARTESIAN_POINT ( 'NONE',  ( 0.000000000000000000, 0.000000000000000000, 27.50000000000000355 ) ) ;
#6020 = CARTESIAN_POINT ( 'NONE',  ( 0.2247925377430787797, -28.49955466461978304, 1.499648419317237913 ) ) ;
#6021 = ADVANCED_FACE ( 'NONE', ( #533 ), #6457, .T. ) ;
#6022 = ORIENTED_EDGE ( 'NONE', *, *, #8947, .T. ) ;
#6023 = ORIENTED_EDGE ( 'NONE', *, *, #3633, .T. ) ;
#6024 = VECTOR ( 'NONE', #2165, 1000.000000000000114 ) ;
#6025 = DIRECTION ( 'NONE',  ( 0.000000000000000000, 0.000000000000000000, -1.000000000000000000 ) ) ;
#6026 = DIRECTION ( 'NONE',  ( -0.000000000000000000, 1.000000000000000000, -0.000000000000000000 ) ) ;
#6027 = EDGE_CURVE ( 'NONE', #7651, #651, #7431, .T. ) ;
#6028 = AXIS2_PLACEMENT_3D ( 'NONE', #5541, #1108, #2755 ) ;
#6029 = CARTESIAN_POINT ( 'NONE',  ( 27.00000000000000355, -34.99999999999999289, 0.000000000000000000 ) ) ;
#6030 = DIRECTION ( 'NONE',  ( 1.000000000000000000, 0.000000000000000000, 0.000000000000000000 ) ) ;
#6031 = ORIENTED_EDGE ( 'NONE', *, *, #4335, .F. ) ;
#6032 = ORIENTED_EDGE ( 'NONE', *, *, #2518, .T. ) ;
#6033 = ORIENTED_EDGE ( 'NONE', *, *, #2964, .T. ) ;
#6034 =( NAMED_UNIT ( * ) SI_UNIT ( $, .STERADIAN. ) SOLID_ANGLE_UNIT ( ) );
#6035 = CIRCLE ( 'NONE', #1884, 13.66147716702868031 ) ;
#6036 = ORIENTED_EDGE ( 'NONE', *, *, #6671, .F. ) ;
#6037 = DIRECTION ( 'NONE',  ( 0.000000000000000000, 0.000000000000000000, 1.000000000000000000 ) ) ;
#6038 = DIRECTION ( 'NONE',  ( 0.000000000000000000, 0.000000000000000000, -1.000000000000000000 ) ) ;
#6039 = DIRECTION ( 'NONE',  ( 1.000000000000000000, 0.000000000000000000, 0.000000000000000000 ) ) ;
#6040 = DIRECTION ( 'NONE',  ( 0.000000000000000000, 0.000000000000000000, 1.000000000000000000 ) ) ;
#6041 = DIRECTION ( 'NONE',  ( 0.000000000000000000, 0.000000000000000000, -1.000000000000000000 ) ) ;
#6042 = CARTESIAN_POINT ( 'NONE',  ( 26.78965207131484050, -6.193975265304529465, 0.4897763315595429767 ) ) ;
#6043 = EDGE_CURVE ( 'NONE', #2947, #6912, #336, .T. ) ;
#6044 = VERTEX_POINT ( 'NONE', #4955 ) ;
#6045 = VERTEX_POINT ( 'NONE', #489 ) ;
#6046 = LINE ( 'NONE', #3158, #8232 ) ;
#6047 = EDGE_LOOP ( 'NONE', ( #5771, #3525, #3817, #978 ) ) ;
#6048 = FACE_BOUND ( 'NONE', #2534, .T. ) ;
#6049 = LINE ( 'NONE', #796, #2742 ) ;
#6050 = ORIENTED_EDGE ( 'NONE', *, *, #1554, .T. ) ;
#6051 = AXIS2_PLACEMENT_3D ( 'NONE', #227, #6093, #2445 ) ;
#6052 = ADVANCED_FACE ( 'NONE', ( #7886 ), #8655, .F. ) ;
#6053 = CARTESIAN_POINT ( 'NONE',  ( 1.335553917663280021, 28.68463450227767453, 1.707979322892793306 ) ) ;
#6054 = VECTOR ( 'NONE', #4367, 1000.000000000000000 ) ;
#6055 = DIRECTION ( 'NONE',  ( -1.000000000000000000, 0.000000000000000000, 0.000000000000000000 ) ) ;
#6056 = PRODUCT_DEFINITION_CONTEXT ( 'detailed design', #499, 'design' ) ;
#6057 = DIRECTION ( 'NONE',  ( -1.000000000000000000, 0.000000000000000000, 0.000000000000000000 ) ) ;
#6058 = ORIENTED_EDGE ( 'NONE', *, *, #9056, .T. ) ;
#6059 = ORIENTED_EDGE ( 'NONE', *, *, #6304, .T. ) ;
#6060 = DIRECTION ( 'NONE',  ( 1.000000000000000000, -1.234117107037592617E-16, -1.075581330716665389E-16 ) ) ;
#6061 = CIRCLE ( 'NONE', #5903, 28.00000000000000711 ) ;
#6062 = DIRECTION ( 'NONE',  ( -1.000000000000000000, 0.000000000000000000, 0.000000000000000000 ) ) ;
#6063 = DIRECTION ( 'NONE',  ( 0.7071067811865494601, -0.4999999999999988343, 0.4999999999999985012 ) ) ;
#6064 = AXIS2_PLACEMENT_3D ( 'NONE', #3775, #6715, #132 ) ;
#6065 = PRODUCT_DEFINITION_CONTEXT ( 'detailed design', #1678, 'design' ) ;
#6066 = FACE_BOUND ( 'NONE', #4564, .T. ) ;
#6067 =( NAMED_UNIT ( * ) PLANE_ANGLE_UNIT ( ) SI_UNIT ( $, .RADIAN. ) );
#6068 = DIRECTION ( 'NONE',  ( -1.000000000000000000, -0.000000000000000000, -0.000000000000000000 ) ) ;
#6069 = PRODUCT_DEFINITION ( 'UNKNOWN', '', #8063, #8925 ) ;
#6070 = ADVANCED_FACE ( 'NONE', ( #7983 ), #1934, .F. ) ;
#6071 = CARTESIAN_POINT ( 'NONE',  ( 0.000000000000000000, 0.000000000000000000, 26.99999999999999289 ) ) ;
#6072 = ADVANCED_FACE ( 'NONE', ( #585 ), #1299, .F. ) ;
#6073 = ORIENTED_EDGE ( 'NONE', *, *, #7823, .F. ) ;
#6074 = CARTESIAN_POINT ( 'NONE',  ( 0.000000000000000000, -34.99999999999999289, 13.50000000000001243 ) ) ;
#6075 = ORIENTED_EDGE ( 'NONE', *, *, #7667, .F. ) ;
#6076 = CARTESIAN_POINT ( 'NONE',  ( 0.000000000000000000, 0.000000000000000000, 25.00000000000000000 ) ) ;
#6077 = CARTESIAN_POINT ( 'NONE',  ( 53.29490495164537833, -15.90990257669733943, -54.09009742330271564 ) ) ;
#6078=STYLED_ITEM('',(#9529),#4990);
#6079 = PLANE ( 'NONE',  #1203 ) ;
#6080 = CARTESIAN_POINT ( 'NONE',  ( 4.000000000000000000, 18.47759065022580316, -8.403668647301632433 ) ) ;
#6081 = EDGE_LOOP ( 'NONE', ( #2451, #2417, #3147, #7597, #7460, #4525, #9046, #2631, #7154, #7868, #8396, #6861, #2740, #4864, #7734, #6969, #6181, #5466, #8275, #2349 ) ) ;
#6082 = VERTEX_POINT ( 'NONE', #632 ) ;
#6083 = AXIS2_PLACEMENT_3D ( 'NONE', #3466, #7036, #7119 ) ;
#6084 = VERTEX_POINT ( 'NONE', #7257 ) ;
#6085 = ORIENTED_EDGE ( 'NONE', *, *, #7638, .F. ) ;
#6086 = CARTESIAN_POINT ( 'NONE',  ( 4.000000000000000000, -20.00000000000120437, 1.560000000004989174 ) ) ;
#6087 = CARTESIAN_POINT ( 'NONE',  ( 0.000000000000000000, 22.50000000000000355, 0.000000000000000000 ) ) ;
#6088 = CYLINDRICAL_SURFACE ( 'NONE', #7307, 3.000000000000000444 ) ;
#6089 = LINE ( 'NONE', #3681, #6162 ) ;
#6090 = CIRCLE ( 'NONE', #8377, 6.000000000000001776 ) ;
#6091 = FACE_OUTER_BOUND ( 'NONE', #6799, .T. ) ;
#6092 = DIRECTION ( 'NONE',  ( 0.000000000000000000, 0.000000000000000000, 1.000000000000000000 ) ) ;
#6093 = DIRECTION ( 'NONE',  ( 0.000000000000000000, 0.000000000000000000, 1.000000000000000000 ) ) ;
#6094 = VERTEX_POINT ( 'NONE', #4231 ) ;
#6095 = EDGE_LOOP ( 'NONE', ( #8883, #4114, #2992, #1847 ) ) ;
#6096 = CARTESIAN_POINT ( 'NONE',  ( 22.50000000000000355, 2.356749903719115078E-13, 0.000000000000000000 ) ) ;
#6097 = EDGE_LOOP ( 'NONE', ( #8179, #8596, #8380 ) ) ;
#6098 = CONICAL_SURFACE ( 'NONE', #8686, 6.000000000000001776, 0.7853981633974500554 ) ;
#6099 = FACE_BOUND ( 'NONE', #6400, .T. ) ;
#6100 = DIRECTION ( 'NONE',  ( 1.000000000000000000, 0.000000000000000000, 0.000000000000000000 ) ) ;
#6101 =( GEOMETRIC_REPRESENTATION_CONTEXT ( 3 ) GLOBAL_UNCERTAINTY_ASSIGNED_CONTEXT ( ( #3740 ) ) GLOBAL_UNIT_ASSIGNED_CONTEXT ( ( #8042, #2995, #8146 ) ) REPRESENTATION_CONTEXT ( 'NONE', 'WORKASPACE' ) );
#6102 = ORIENTED_EDGE ( 'NONE', *, *, #4225, .F. ) ;
#6103 =( REPRESENTATION_RELATIONSHIP ('NONE','NONE', #1933, #8501 ) REPRESENTATION_RELATIONSHIP_WITH_TRANSFORMATION ( #7871 )SHAPE_REPRESENTATION_RELATIONSHIP( ) );
#6104 = CARTESIAN_POINT ( 'NONE',  ( 0.000000000000000000, 18.47759065022658120, 6.903668647304224137 ) ) ;
#6105 = VECTOR ( 'NONE', #6934, 1000.000000000000000 ) ;
#6106 = DIRECTION ( 'NONE',  ( -0.000000000000000000, -0.000000000000000000, -1.000000000000000000 ) ) ;
#6107 = CARTESIAN_POINT ( 'NONE',  ( 27.00000000000000355, 35.00000000000000000, 59.00000000000000000 ) ) ;
#6108 = CIRCLE ( 'NONE', #5790, 2.999999999999999112 ) ;
#6109 = ORIENTED_EDGE ( 'NONE', *, *, #4239, .T. ) ;
#6110 = ORIENTED_EDGE ( 'NONE', *, *, #4300, .F. ) ;
#6111 = AXIS2_PLACEMENT_3D ( 'NONE', #8313, #6208, #9123 ) ;
#6112 = CONTEXT_DEPENDENT_SHAPE_REPRESENTATION ( #3942, #3784 ) ;
#6113 = AXIS2_PLACEMENT_3D ( 'NONE', #2930, #6682, #3029 ) ;
#6114 = DIRECTION ( 'NONE',  ( -0.000000000000000000, -0.000000000000000000, -1.000000000000000000 ) ) ;
#6115 = DIRECTION ( 'NONE',  ( 0.000000000000000000, 0.000000000000000000, -1.000000000000000000 ) ) ;
#6116 = AXIS2_PLACEMENT_3D ( 'NONE', #2401, #5332, #5281 ) ;
#6117 = VECTOR ( 'NONE', #5899, 1000.000000000000000 ) ;
#6118 = DIRECTION ( 'NONE',  ( -1.000000000000000000, 0.000000000000000000, 0.000000000000000000 ) ) ;
#6119 = SURFACE_STYLE_USAGE ( .BOTH. , #8361 ) ;
#6120 = ADVANCED_FACE ( 'NONE', ( #3561 ), #6405, .T. ) ;
#6121 = DIRECTION ( 'NONE',  ( 0.000000000000000000, 0.000000000000000000, -1.000000000000000000 ) ) ;
#6122 = ORIENTED_EDGE ( 'NONE', *, *, #7110, .F. ) ;
#6123 = AXIS2_PLACEMENT_3D ( 'NONE', #5756, #464, #606 ) ;
#6124 = VERTEX_POINT ( 'NONE', #8703 ) ;
#6125 = CARTESIAN_POINT ( 'NONE',  ( 0.4999999999999935052, 2.755455298081544778E-15, -22.50000000000000000 ) ) ;
#6126 = LINE ( 'NONE', #2474, #411 ) ;
#6127 = CYLINDRICAL_SURFACE ( 'NONE', #1354, 1.559999999998939346 ) ;
#6128 = EDGE_CURVE ( 'NONE', #313, #7585, #3279, .T. ) ;
#6129 = LINE ( 'NONE', #5450, #5709 ) ;
#6130 = VECTOR ( 'NONE', #6184, 1000.000000000000000 ) ;
#6131 = EDGE_CURVE ( 'NONE', #3020, #2924, #485, .T. ) ;
#6132 = VECTOR ( 'NONE', #8897, 1000.000000000000000 ) ;
#6133 = ORIENTED_EDGE ( 'NONE', *, *, #8122, .T. ) ;
#6134 = EDGE_CURVE ( 'NONE', #438, #5859, #3714, .T. ) ;
#6135 = ADVANCED_FACE ( 'NONE', ( #6685, #4472 ), #6598, .F. ) ;
#6136 = VERTEX_POINT ( 'NONE', #5196 ) ;
#6137 = ORIENTED_EDGE ( 'NONE', *, *, #4011, .F. ) ;
#6138 = SHAPE_REPRESENTATION_RELATIONSHIP ( 'NONE' , 'NONE' ,  #6298, #8060 ) ;
#6139 = ORIENTED_EDGE ( 'NONE', *, *, #7669, .T. ) ;
#6140 = LINE ( 'NONE', #3820, #2595 ) ;
#6141 = CARTESIAN_POINT ( 'NONE',  ( 0.7500000000000000000, -0.7500000000000000000, 1.500000000000000000 ) ) ;
#6142 = LINE ( 'NONE', #7564, #4091 ) ;
#6143 = DIRECTION ( 'NONE',  ( 0.000000000000000000, 0.000000000000000000, -1.000000000000000000 ) ) ;
#6144 = DIRECTION ( 'NONE',  ( 0.000000000000000000, 0.000000000000000000, 1.000000000000000000 ) ) ;
#6145 = CARTESIAN_POINT ( 'NONE',  ( -53.29490495164537833, -11.46446609406728179, -97.50000000000000000 ) ) ;
#6146 = CARTESIAN_POINT ( 'NONE',  ( 28.75000000000002842, -0.6738334415499637187, 1.750000000000026423 ) ) ;
#6147 = ORIENTED_EDGE ( 'NONE', *, *, #823, .T. ) ;
#6148 = VERTEX_POINT ( 'NONE', #8131 ) ;
#6149 = FACE_OUTER_BOUND ( 'NONE', #2591, .T. ) ;
#6150 = ORIENTED_EDGE ( 'NONE', *, *, #1836, .F. ) ;
#6151 = ADVANCED_FACE ( 'NONE', ( #5914 ), #7498, .F. ) ;
#6152 = DIRECTION ( 'NONE',  ( -1.000000000000000000, 0.000000000000000000, 0.000000000000000000 ) ) ;
#6153 = CARTESIAN_POINT ( 'NONE',  ( 0.000000000000000000, -35.00000000000000000, 49.50000000000000000 ) ) ;
#6154 = VERTEX_POINT ( 'NONE', #13 ) ;
#6155 = LINE ( 'NONE', #372, #8150 ) ;
#6156 = EDGE_CURVE ( 'NONE', #3651, #5672, #6017, .T. ) ;
#6157 = DIRECTION ( 'NONE',  ( 1.000000000000000000, 0.000000000000000000, -0.000000000000000000 ) ) ;
#6158 = CARTESIAN_POINT ( 'NONE',  ( 1.687492729851148177, -28.61614266785989358, 1.663948857909935075 ) ) ;
#6159 = ORIENTED_EDGE ( 'NONE', *, *, #6220, .T. ) ;
#6160 = EDGE_LOOP ( 'NONE', ( #3085, #8000 ) ) ;
#6161 = CONTEXT_DEPENDENT_SHAPE_REPRESENTATION ( #3759, #4318 ) ;
#6162 = VECTOR ( 'NONE', #6618, 1000.000000000000000 ) ;
#6163 = LINE ( 'NONE', #2363, #8556 ) ;
#6164 = FACE_OUTER_BOUND ( 'NONE', #4847, .T. ) ;
#6165 = CARTESIAN_POINT ( 'NONE',  ( 1.750000000000001554, 1.749999999999984235, 0.000000000000000000 ) ) ;
#6166 = DIRECTION ( 'NONE',  ( -0.000000000000000000, -0.000000000000000000, -1.000000000000000000 ) ) ;
#6167 = CARTESIAN_POINT ( 'NONE',  ( -28.21952111405550312, 3.291689805591859752, 1.408977859035693170 ) ) ;
#6168 = EDGE_CURVE ( 'NONE', #3913, #5419, #7707, .T. ) ;
#6169 = EDGE_LOOP ( 'NONE', ( #9275, #7341 ) ) ;
#6170 = FILL_AREA_STYLE ('',( #6888 ) ) ;
#6171 = VERTEX_POINT ( 'NONE', #1492 ) ;
#6172 = LINE ( 'NONE', #9082, #1878 ) ;
#6173 = CIRCLE ( 'NONE', #4935, 3.000000000000000000 ) ;
#6174 = CARTESIAN_POINT ( 'NONE',  ( 5.000000000000000000, 14.14213562373247868, 14.14213562373282329 ) ) ;
#6175 = ADVANCED_FACE ( 'NONE', ( #917 ), #7396, .F. ) ;
#6176 = DIRECTION ( 'NONE',  ( 0.000000000000000000, 0.000000000000000000, 1.000000000000000000 ) ) ;
#6177 = DIRECTION ( 'NONE',  ( 0.000000000000000000, 0.7071067811865473507, 0.7071067811865477948 ) ) ;
#6178 = ORIENTED_EDGE ( 'NONE', *, *, #5673, .T. ) ;
#6179 = VECTOR ( 'NONE', #5737, 1000.000000000000000 ) ;
#6180 = VERTEX_POINT ( 'NONE', #159 ) ;
#6181 = ORIENTED_EDGE ( 'NONE', *, *, #4113, .T. ) ;
#6182 =( NAMED_UNIT ( * ) PLANE_ANGLE_UNIT ( ) SI_UNIT ( $, .RADIAN. ) );
#6183 = ORIENTED_EDGE ( 'NONE', *, *, #4183, .F. ) ;
#6184 = DIRECTION ( 'NONE',  ( -0.000000000000000000, -0.000000000000000000, 1.000000000000000000 ) ) ;
#6185 = DIRECTION ( 'NONE',  ( 0.000000000000000000, 0.000000000000000000, 1.000000000000000000 ) ) ;
#6186 = CARTESIAN_POINT ( 'NONE',  ( 0.000000000000000000, 0.000000000000000000, 25.00000000000000000 ) ) ;
#6187 = CARTESIAN_POINT ( 'NONE',  ( -37.22467645238203460, -47.05659850664382304, -5.608807313787673721 ) ) ;
#6188 = CARTESIAN_POINT ( 'NONE',  ( 3.000000000000000000, -22.50000000000000355, 10.00000000000000000 ) ) ;
#6189 = CIRCLE ( 'NONE', #9395, 59.00000000000000000 ) ;
#6190 = FACE_OUTER_BOUND ( 'NONE', #2309, .T. ) ;
#6191 = VERTEX_POINT ( 'NONE', #8937 ) ;
#6192 = ORIENTED_EDGE ( 'NONE', *, *, #1615, .T. ) ;
#6193 = DIRECTION ( 'NONE',  ( 0.000000000000000000, 0.000000000000000000, -1.000000000000000000 ) ) ;
#6194 = ORIENTED_EDGE ( 'NONE', *, *, #5553, .F. ) ;
#6195 = EDGE_CURVE ( 'NONE', #8143, #4833, #4430, .T. ) ;
#6196 = FACE_BOUND ( 'NONE', #7561, .T. ) ;
#6197 = ORIENTED_EDGE ( 'NONE', *, *, #9343, .F. ) ;
#6198 = CARTESIAN_POINT ( 'NONE',  ( 2.749999999999996447, -0.7500000000000000000, 0.000000000000000000 ) ) ;
#6199 = CIRCLE ( 'NONE', #3121, 26.99999999999997868 ) ;
#6200 = VECTOR ( 'NONE', #1812, 1000.000000000000114 ) ;
#6201 = LINE ( 'NONE', #9022, #8195 ) ;
#6202 = CARTESIAN_POINT ( 'NONE',  ( 0.000000000000000000, 0.000000000000000000, 10.00000000000000000 ) ) ;
#6203 = ORIENTED_EDGE ( 'NONE', *, *, #3975, .T. ) ;
#6204 = ORIENTED_EDGE ( 'NONE', *, *, #4434, .T. ) ;
#6205 = SHAPE_DEFINITION_REPRESENTATION ( #3703, #1625 ) ;
#6206 = DIRECTION ( 'NONE',  ( 0.000000000000000000, 0.000000000000000000, 1.000000000000000000 ) ) ;
#6207 = CARTESIAN_POINT ( 'NONE',  ( 51.96152422706632734, -30.00000000000000000, -80.85015119857384036 ) ) ;
#6208 = DIRECTION ( 'NONE',  ( -1.000000000000000000, -0.000000000000000000, -0.000000000000000000 ) ) ;
#6209 = CARTESIAN_POINT ( 'NONE',  ( 0.000000000000000000, 0.000000000000000000, 0.000000000000000000 ) ) ;
#6210 = ORIENTED_EDGE ( 'NONE', *, *, #9052, .F. ) ;
#6211 = VECTOR ( 'NONE', #2642, 1000.000000000000000 ) ;
#6212 = FACE_OUTER_BOUND ( 'NONE', #717, .T. ) ;
#6213 = ORIENTED_EDGE ( 'NONE', *, *, #2469, .T. ) ;
#6214 = DIRECTION ( 'NONE',  ( 0.000000000000000000, 0.000000000000000000, 1.000000000000000000 ) ) ;
#6215 = CIRCLE ( 'NONE', #7118, 17.50000000000000000 ) ;
#6216 = DIRECTION ( 'NONE',  ( 0.000000000000000000, 0.000000000000000000, 1.000000000000000000 ) ) ;
#6217 = CARTESIAN_POINT ( 'NONE',  ( 17.50000000000000355, 0.000000000000000000, 14.49999999999999822 ) ) ;
#6218 = EDGE_CURVE ( 'NONE', #5331, #3688, #4330, .T. ) ;
#6219 = DIRECTION ( 'NONE',  ( 0.000000000000000000, 0.000000000000000000, -1.000000000000000000 ) ) ;
#6220 = EDGE_CURVE ( 'NONE', #4781, #2503, #8217, .T. ) ;
#6221 = VECTOR ( 'NONE', #2465, 1000.000000000000114 ) ;
#6222 =( REPRESENTATION_RELATIONSHIP ('NONE','NONE', #1933, #8501 ) REPRESENTATION_RELATIONSHIP_WITH_TRANSFORMATION ( #2151 )SHAPE_REPRESENTATION_RELATIONSHIP( ) );
#6223 = EDGE_LOOP ( 'NONE', ( #1450, #704 ) ) ;
#6224 = ADVANCED_FACE ( 'NONE', ( #1640 ), #5869, .F. ) ;
#6225 = ORIENTED_EDGE ( 'NONE', *, *, #5966, .T. ) ;
#6226 = VERTEX_POINT ( 'NONE', #8027 ) ;
#6227 = CARTESIAN_POINT ( 'NONE',  ( -34.25000000000000000, -43.00000000000000000, 25.00000000000000000 ) ) ;
#6228 = DIRECTION ( 'NONE',  ( 0.000000000000000000, 0.000000000000000000, -1.000000000000000000 ) ) ;
#6229 = DIRECTION ( 'NONE',  ( -0.000000000000000000, -0.000000000000000000, -1.000000000000000000 ) ) ;
#6230 = CARTESIAN_POINT ( 'NONE',  ( 32.00000000000000711, 0.000000000000000000, 32.00000000000000000 ) ) ;
#6231 = DIRECTION ( 'NONE',  ( -1.000000000000000000, 0.000000000000000000, 0.000000000000000000 ) ) ;
#6232 =( BOUNDED_CURVE ( )  B_SPLINE_CURVE ( 3, ( #2443, #1566, #3006, #8246 ),
 .UNSPECIFIED., .F., .T. ) 
 B_SPLINE_CURVE_WITH_KNOTS ( ( 4, 4 ),
 ( 2.356194490192344837, 3.141592653589793116 ),
 .UNSPECIFIED. ) 
 CURVE ( )  GEOMETRIC_REPRESENTATION_ITEM ( )  RATIONAL_B_SPLINE_CURVE ( ( 1.000000000000000000, 0.9492530216741911220, 0.9492530216741911220, 1.000000000000000000 ) ) 
 REPRESENTATION_ITEM ( '' )  );
#6233 = DIRECTION ( 'NONE',  ( 0.000000000000000000, 0.000000000000000000, -1.000000000000000000 ) ) ;
#6234 = EDGE_CURVE ( 'NONE', #1975, #6538, #4030, .T. ) ;
#6235 = ORIENTED_EDGE ( 'NONE', *, *, #7859, .F. ) ;
#6236 = ORIENTED_EDGE ( 'NONE', *, *, #3281, .F. ) ;
#6237 =( BOUNDED_CURVE ( )  B_SPLINE_CURVE ( 3, ( #9250, #3489, #9352, #4078 ),
 .UNSPECIFIED., .F., .F. ) 
 B_SPLINE_CURVE_WITH_KNOTS ( ( 4, 4 ),
 ( 5.497787143782137953, 6.283185307179586232 ),
 .UNSPECIFIED. ) 
 CURVE ( )  GEOMETRIC_REPRESENTATION_ITEM ( )  RATIONAL_B_SPLINE_CURVE ( ( 1.000000000000000000, 0.9492530216741911220, 0.9492530216741911220, 1.000000000000000000 ) ) 
 REPRESENTATION_ITEM ( '' )  );
#6238 = CARTESIAN_POINT ( 'NONE',  ( 60.00000000000000000, 15.90990257669733943, -85.90990257669729147 ) ) ;
#6239 = VERTEX_POINT ( 'NONE', #813 ) ;
#6240 = CARTESIAN_POINT ( 'NONE',  ( 0.000000000000000000, 0.000000000000000000, 5.000000000000000000 ) ) ;
#6241 = DIRECTION ( 'NONE',  ( -1.000000000000000000, 0.000000000000000000, 0.000000000000000000 ) ) ;
#6242 = ORIENTED_EDGE ( 'NONE', *, *, #6522, .F. ) ;
#6243 = CIRCLE ( 'NONE', #546, 22.00000000000000355 ) ;
#6244 = AXIS2_PLACEMENT_3D ( 'NONE', #5328, #6913, #9151 ) ;
#6245 = CARTESIAN_POINT ( 'NONE',  ( 31.00000000000002132, 2.143131898507868643E-15, 49.50000000000000000 ) ) ;
#6246 = EDGE_CURVE ( 'NONE', #6332, #5476, #4573, .T. ) ;
#6247 = CARTESIAN_POINT ( 'NONE',  ( 0.7500000000000000000, -0.7500000000000000000, 0.000000000000000000 ) ) ;
#6248 = DIRECTION ( 'NONE',  ( 0.000000000000000000, 0.000000000000000000, 1.000000000000000000 ) ) ;
#6249 = CIRCLE ( 'NONE', #2091, 2.999999999999999556 ) ;
#6250 = EDGE_CURVE ( 'NONE', #602, #4565, #4793, .T. ) ;
#6251 = VERTEX_POINT ( 'NONE', #5246 ) ;
#6252 = VECTOR ( 'NONE', #3206, 1000.000000000000114 ) ;
#6253 = ORIENTED_EDGE ( 'NONE', *, *, #3731, .F. ) ;
#6254 = EDGE_CURVE ( 'NONE', #4422, #7550, #8748, .T. ) ;
#6255 = ADVANCED_FACE ( 'NONE', ( #1587 ), #770, .F. ) ;
#6256 = APPLICATION_PROTOCOL_DEFINITION ( 'draft international standard', 'automotive_design', 1998, #6585 ) ;
#6257 = FACE_OUTER_BOUND ( 'NONE', #8443, .T. ) ;
#6258 = AXIS2_PLACEMENT_3D ( 'NONE', #6274, #1296, #7071 ) ;
#6259 = EDGE_CURVE ( 'NONE', #6631, #2159, #9384, .T. ) ;
#6260 = DIRECTION ( 'NONE',  ( 1.000000000000000000, 0.000000000000000000, 0.000000000000000000 ) ) ;
#6261 = AXIS2_PLACEMENT_3D ( 'NONE', #7888, #634, #2760 ) ;
#6262 = CARTESIAN_POINT ( 'NONE',  ( 28.50000000000000355, 7.347880794884122694E-16, 2.000000000000035083 ) ) ;
#6263 = EDGE_CURVE ( 'NONE', #8518, #8127, #3223, .T. ) ;
#6264 = FACE_OUTER_BOUND ( 'NONE', #1989, .T. ) ;
#6265 = VECTOR ( 'NONE', #3086, 1000.000000000000114 ) ;
#6266 = EDGE_CURVE ( 'NONE', #6389, #8082, #3101, .T. ) ;
#6267 = EDGE_LOOP ( 'NONE', ( #8392, #9059 ) ) ;
#6268 = CIRCLE ( 'NONE', #3336, 18.50000000000001776 ) ;
#6269 = CARTESIAN_POINT ( 'NONE',  ( -53.29490495164537833, -27.56180520566615044, -81.40266088840114378 ) ) ;
#6270 = VERTEX_POINT ( 'NONE', #6207 ) ;
#6271 = EDGE_CURVE ( 'NONE', #4522, #7415, #1098, .T. ) ;
#6272 = CIRCLE ( 'NONE', #1336, 5.000000000000000888 ) ;
#6273 = DIRECTION ( 'NONE',  ( 1.000000000000000000, 0.000000000000000000, 0.000000000000000000 ) ) ;
#6274 = CARTESIAN_POINT ( 'NONE',  ( 0.000000000000000000, 0.000000000000000000, 20.00000000000000000 ) ) ;
#6275 = AXIS2_PLACEMENT_3D ( 'NONE', #1725, #5336, #241 ) ;
#6276 = CARTESIAN_POINT ( 'NONE',  ( 1.750000000000015987, 1.749999999999999778, 0.000000000000000000 ) ) ;
#6277 = AXIS2_PLACEMENT_3D ( 'NONE', #1872, #4801, #4850 ) ;
#6278 = CARTESIAN_POINT ( 'NONE',  ( 53.29490495164537833, -27.56180520566615044, -134.0000000000000284 ) ) ;
#6279 = VERTEX_POINT ( 'NONE', #1101 ) ;
#6280 = EDGE_LOOP ( 'NONE', ( #4101, #9325 ) ) ;
#6281 = CARTESIAN_POINT ( 'NONE',  ( 70.51394605043111596, 64.54333883337996269, 59.86606487507562946 ) ) ;
#6282 = ORIENTED_EDGE ( 'NONE', *, *, #753, .T. ) ;
#6283 = DIRECTION ( 'NONE',  ( -1.000000000000000000, 0.000000000000000000, 0.000000000000000000 ) ) ;
#6284 = CARTESIAN_POINT ( 'NONE',  ( 30.00000000000000000, 3.673940397442059178E-15, 10.00000000000000000 ) ) ;
#6285 = TOROIDAL_SURFACE ( 'NONE', #4433, 5.000000000000000888, 1.000000000000000000 ) ;
#6286 = CARTESIAN_POINT ( 'NONE',  ( -1.750000000000001554, -1.749999999999984235, 0.000000000000000000 ) ) ;
#6287 = AXIS2_PLACEMENT_3D ( 'NONE', #6597, #7301, #6683 ) ;
#6288 = CARTESIAN_POINT ( 'NONE',  ( -41.99999999999999289, -12.49999999999999645, -100.0000000000000000 ) ) ;
#6289 = ORIENTED_EDGE ( 'NONE', *, *, #6758, .F. ) ;
#6290 = VERTEX_POINT ( 'NONE', #7643 ) ;
#6291 = CARTESIAN_POINT ( 'NONE',  ( 0.000000000000000000, -9.628187502531647418E-13, -18.43999999999823913 ) ) ;
#6292 = ORIENTED_EDGE ( 'NONE', *, *, #5844, .T. ) ;
#6293 = CARTESIAN_POINT ( 'NONE',  ( -19.50000000000000000, -7.819093608422630136E-14, 5.000000000000000000 ) ) ;
#6294 = CARTESIAN_POINT ( 'NONE',  ( -37.00000000000000711, 15.90990257669733943, -54.09009742330271564 ) ) ;
#6295 = ORIENTED_EDGE ( 'NONE', *, *, #3709, .T. ) ;
#6296 = CARTESIAN_POINT ( 'NONE',  ( -8.000000000000021316, 22.50000000000000355, 0.000000000000000000 ) ) ;
#6297 = LINE ( 'NONE', #9201, #4008 ) ;
#6298 = SHAPE_REPRESENTATION ( '4-Axle(Cross)', ( #1614 ), #1322 ) ;
#6299 = FACE_OUTER_BOUND ( 'NONE', #1073, .T. ) ;
#6300 = DIRECTION ( 'NONE',  ( -1.000000000000000000, 0.000000000000000000, 0.000000000000000000 ) ) ;
#6301 = EDGE_LOOP ( 'NONE', ( #5326, #8722, #8975, #237 ) ) ;
#6302 = ORIENTED_EDGE ( 'NONE', *, *, #6246, .T. ) ;
#6303 = DIRECTION ( 'NONE',  ( 0.000000000000000000, 0.000000000000000000, -1.000000000000000000 ) ) ;
#6304 = EDGE_CURVE ( 'NONE', #9386, #3367, #3558, .T. ) ;
#6305 = EDGE_CURVE ( 'NONE', #367, #7733, #6974, .T. ) ;
#6306 = DIRECTION ( 'NONE',  ( -1.000000000000000000, 0.000000000000000000, 0.000000000000000000 ) ) ;
#6307 = CARTESIAN_POINT ( 'NONE',  ( 15.70011763207404876, -9.048619709455115512, 16.29988236792595302 ) ) ;
#6308 = FACE_OUTER_BOUND ( 'NONE', #8517, .T. ) ;
#6309 = MANIFOLD_SOLID_BREP ( 'Pah2', #5165 ) ;
#6310 = ORIENTED_EDGE ( 'NONE', *, *, #2125, .T. ) ;
#6311 = ORIENTED_EDGE ( 'NONE', *, *, #7358, .T. ) ;
#6312 = CONICAL_SURFACE ( 'NONE', #8899, 11.96410161513786008, 0.2617993877991461882 ) ;
#6313 = ORIENTED_EDGE ( 'NONE', *, *, #3258, .F. ) ;
#6314 = DIRECTION ( 'NONE',  ( 1.000000000000000000, -0.000000000000000000, -0.000000000000000000 ) ) ;
#6315 = CARTESIAN_POINT ( 'NONE',  ( -26.99999999999996092, 29.99999999999997158, 0.000000000000000000 ) ) ;
#6316 = CARTESIAN_POINT ( 'NONE',  ( -2.999999999999842792, -22.50000000000000355, 10.00000000000000000 ) ) ;
#6317 = CARTESIAN_POINT ( 'NONE',  ( -31.99999999999999289, -34.99999999999999289, 5.000000000000004441 ) ) ;
#6318 = DIRECTION ( 'NONE',  ( -0.7071067811865479058, 8.659560562354937789E-17, 0.7071067811865471286 ) ) ;
#6319 = ORIENTED_EDGE ( 'NONE', *, *, #9144, .F. ) ;
#6320 = EDGE_LOOP ( 'NONE', ( #170, #8927 ) ) ;
#6321 = CARTESIAN_POINT ( 'NONE',  ( 7.219041098785710986, 116.4430730160533898, 43.10058005594827790 ) ) ;
#6322 = ORIENTED_EDGE ( 'NONE', *, *, #5711, .T. ) ;
#6323 = CARTESIAN_POINT ( 'NONE',  ( -16.00000000000000000, 1.959434878635765131E-15, 11.00000000000000000 ) ) ;
#6324 = DIRECTION ( 'NONE',  ( 1.000000000000000000, 0.000000000000000000, 0.000000000000000000 ) ) ;
#6325 = CARTESIAN_POINT ( 'NONE',  ( 0.7500000000000000000, -0.7500000000000000000, 1.500000000000000000 ) ) ;
#6326 = DIRECTION ( 'NONE',  ( -0.000000000000000000, -0.000000000000000000, -1.000000000000000000 ) ) ;
#6327 = AXIS2_PLACEMENT_3D ( 'NONE', #3417, #3512, #5004 ) ;
#6328 = DIRECTION ( 'NONE',  ( -1.000000000000000000, 0.000000000000000000, 0.000000000000000000 ) ) ;
#6329 = ORIENTED_EDGE ( 'NONE', *, *, #4862, .F. ) ;
#6330 = ORIENTED_EDGE ( 'NONE', *, *, #4953, .F. ) ;
#6331 = DIRECTION ( 'NONE',  ( -1.000000000000000000, 0.000000000000000000, 0.000000000000000000 ) ) ;
#6332 = VERTEX_POINT ( 'NONE', #5532 ) ;
#6333 = CARTESIAN_POINT ( 'NONE',  ( -26.99999999999997513, -32.49999999999997868, 2.500000000000002220 ) ) ;
#6334 = CARTESIAN_POINT ( 'NONE',  ( 0.000000000000000000, 1.673048428422632513E-15, -13.66147716702868031 ) ) ;
#6335 = DIRECTION ( 'NONE',  ( 0.7071067811865505703, 0.7071067811865444641, -0.000000000000000000 ) ) ;
#6336 = DIRECTION ( 'NONE',  ( 0.000000000000000000, 0.000000000000000000, -1.000000000000000000 ) ) ;
#6337 = AXIS2_PLACEMENT_3D ( 'NONE', #4228, #8601, #6273 ) ;
#6338 = EDGE_CURVE ( 'NONE', #7970, #2895, #3997, .T. ) ;
#6339 = DIRECTION ( 'NONE',  ( 1.000000000000000000, 0.000000000000000000, 0.000000000000000000 ) ) ;
#6340 = ORIENTED_EDGE ( 'NONE', *, *, #194, .T. ) ;
#6341 = ORIENTED_EDGE ( 'NONE', *, *, #4163, .T. ) ;
#6342 = ADVANCED_FACE ( 'NONE', ( #2466 ), #4086, .F. ) ;
#6343 = ITEM_DEFINED_TRANSFORMATION ( 'NONE', 'NONE', #2079,  #1614 ) ;
#6344 = AXIS2_PLACEMENT_3D ( 'NONE', #4241, #7038, #9329 ) ;
#6345 = FACE_OUTER_BOUND ( 'NONE', #1597, .T. ) ;
#6346 = CARTESIAN_POINT ( 'NONE',  ( 17.49999999999999645, -4.703319286132086496, 14.49999999999999822 ) ) ;
#6347 = DIRECTION ( 'NONE',  ( 1.000000000000000000, 0.000000000000000000, -0.000000000000000000 ) ) ;
#6348 = MANIFOLD_SOLID_BREP ( 'Pah3', #1644 ) ;
#6349 = ORIENTED_EDGE ( 'NONE', *, *, #1008, .T. ) ;
#6350 = ORIENTED_EDGE ( 'NONE', *, *, #2430, .F. ) ;
#6351 = ORIENTED_EDGE ( 'NONE', *, *, #1288, .F. ) ;
#6352 = ORIENTED_EDGE ( 'NONE', *, *, #7741, .F. ) ;
#6353 = CARTESIAN_POINT ( 'NONE',  ( -28.50000000000000000, -7.855833012397050680E-14, 5.000000000000000000 ) ) ;
#6354 = CARTESIAN_POINT ( 'NONE',  ( -38.00000000000000711, -43.00000000000000000, -7.366666666666667140 ) ) ;
#6355 = DIRECTION ( 'NONE',  ( -1.000000000000000000, 0.000000000000000000, -0.000000000000000000 ) ) ;
#6356 = EDGE_CURVE ( 'NONE', #991, #2334, #6049, .T. ) ;
#6357 = CARTESIAN_POINT ( 'NONE',  ( 4.000000000000000888, 0.000000000000000000, 0.000000000000000000 ) ) ;
#6358 = EDGE_CURVE ( 'NONE', #4565, #9386, #5127, .T. ) ;
#6359 = ADVANCED_FACE ( 'NONE', ( #3641 ), #6730, .F. ) ;
#6360 = AXIS2_PLACEMENT_3D ( 'NONE', #760, #5283, #8828 ) ;
#6361 = DIRECTION ( 'NONE',  ( -0.000000000000000000, 0.000000000000000000, 1.000000000000000000 ) ) ;
#6362 = VERTEX_POINT ( 'NONE', #2297 ) ;
#6363 = ORIENTED_EDGE ( 'NONE', *, *, #6943, .T. ) ;
#6364 = AXIS2_PLACEMENT_3D ( 'NONE', #5893, #8818, #8152 ) ;
#6365 = CARTESIAN_POINT ( 'NONE',  ( 7.219041098785710986, 48.46227998254432379, 44.71667984720244249 ) ) ;
#6366 = EDGE_CURVE ( 'NONE', #956, #3327, #1621, .T. ) ;
#6367 = VERTEX_POINT ( 'NONE', #1572 ) ;
#6368 = CARTESIAN_POINT ( 'NONE',  ( 0.000000000000000000, -7.653668647303860872, -18.47759065022490432 ) ) ;
#6369 = DIRECTION ( 'NONE',  ( 0.7071067811865463515, 0.000000000000000000, 0.7071067811865487940 ) ) ;
#6370 = VECTOR ( 'NONE', #3634, 999.9999999999998863 ) ;
#6371 = DIRECTION ( 'NONE',  ( 0.000000000000000000, 0.000000000000000000, -1.000000000000000000 ) ) ;
#6372 = AXIS2_PLACEMENT_3D ( 'NONE', #1972, #4941, #8549 ) ;
#6373 = EDGE_CURVE ( 'NONE', #8783, #7512, #3832, .T. ) ;
#6374 = DIRECTION ( 'NONE',  ( -0.7071067811865461294, -0.7071067811865489050, -3.776607970617559778E-15 ) ) ;
#6375 = DIRECTION ( 'NONE',  ( 0.000000000000000000, 0.000000000000000000, 1.000000000000000000 ) ) ;
#6376 = ORIENTED_EDGE ( 'NONE', *, *, #192, .F. ) ;
#6377 = EDGE_CURVE ( 'NONE', #4466, #7912, #8917, .T. ) ;
#6378 = ORIENTED_EDGE ( 'NONE', *, *, #8231, .T. ) ;
#6379 = CARTESIAN_POINT ( 'NONE',  ( -4.078200081724630444, 26.91636876093601316, 0.2219739674467013368 ) ) ;
#6380 = ORIENTED_EDGE ( 'NONE', *, *, #4958, .F. ) ;
#6381 = DIRECTION ( 'NONE',  ( 0.000000000000000000, 0.000000000000000000, -1.000000000000000000 ) ) ;
#6382 = CARTESIAN_POINT ( 'NONE',  ( 27.00000000000000000, -43.00000000000000000, 11.99999999999999645 ) ) ;
#6383 = FACE_OUTER_BOUND ( 'NONE', #8708, .T. ) ;
#6384 = DIRECTION ( 'NONE',  ( 0.000000000000000000, 0.000000000000000000, -1.000000000000000000 ) ) ;
#6385 =( GEOMETRIC_REPRESENTATION_CONTEXT ( 3 ) GLOBAL_UNCERTAINTY_ASSIGNED_CONTEXT ( ( #5284 ) ) GLOBAL_UNIT_ASSIGNED_CONTEXT ( ( #2436, #6182, #9090 ) ) REPRESENTATION_CONTEXT ( 'NONE', 'WORKASPACE' ) );
#6386 = CARTESIAN_POINT ( 'NONE',  ( 0.000000000000000000, -7.653668647301985040, 17.72759065022987812 ) ) ;
#6387 = CARTESIAN_POINT ( 'NONE',  ( -6.193323906411744240, -26.79012200670185351, 0.4900784328797758715 ) ) ;
#6388 = EDGE_LOOP ( 'NONE', ( #3049, #7616, #5864, #5782 ) ) ;
#6389 = VERTEX_POINT ( 'NONE', #8113 ) ;
#6390 = AXIS2_PLACEMENT_3D ( 'NONE', #3602, #8074, #8789 ) ;
#6391 = ITEM_DEFINED_TRANSFORMATION ( 'NONE', 'NONE', #6849,  #1614 ) ;
#6392 = PRODUCT_DEFINITION_SHAPE ( 'NONE', 'NONE',  #9493 ) ;
#6393 = DIRECTION ( 'NONE',  ( -0.000000000000000000, -0.000000000000000000, -1.000000000000000000 ) ) ;
#6394 = VECTOR ( 'NONE', #5217, 999.9999999999998863 ) ;
#6395 = FACE_OUTER_BOUND ( 'NONE', #8821, .T. ) ;
#6396 = CARTESIAN_POINT ( 'NONE',  ( 27.00000000000000000, 43.00000000000000000, -25.00000000000000000 ) ) ;
#6397 = ORIENTED_EDGE ( 'NONE', *, *, #6458, .F. ) ;
#6398 = ORIENTED_EDGE ( 'NONE', *, *, #895, .F. ) ;
#6399 = ORIENTED_EDGE ( 'NONE', *, *, #6950, .F. ) ;
#6400 = EDGE_LOOP ( 'NONE', ( #1408, #471 ) ) ;
#6401 = VECTOR ( 'NONE', #7599, 1000.000000000000000 ) ;
#6402 = DIRECTION ( 'NONE',  ( 0.000000000000000000, 0.000000000000000000, -1.000000000000000000 ) ) ;
#6403 = DIRECTION ( 'NONE',  ( -0.000000000000000000, -0.000000000000000000, -1.000000000000000000 ) ) ;
#6404 = DIRECTION ( 'NONE',  ( 0.000000000000000000, 0.000000000000000000, -1.000000000000000000 ) ) ;
#6405 = PLANE ( 'NONE',  #8771 ) ;
#6406 = AXIS2_PLACEMENT_3D ( 'NONE', #1068, #2515, #4049 ) ;
#6407 = FACE_OUTER_BOUND ( 'NONE', #6959, .T. ) ;
#6408 = VERTEX_POINT ( 'NONE', #4557 ) ;
#6409 = DIRECTION ( 'NONE',  ( -0.000000000000000000, -0.000000000000000000, -1.000000000000000000 ) ) ;
#6410 = DIRECTION ( 'NONE',  ( 0.000000000000000000, -0.5535840618632023036, -0.8327933035579949683 ) ) ;
#6411 = ORIENTED_EDGE ( 'NONE', *, *, #598, .T. ) ;
#6412 = CIRCLE ( 'NONE', #575, 1.559999999998939346 ) ;
#6413 = PLANE ( 'NONE',  #8328 ) ;
#6414 = CIRCLE ( 'NONE', #6880, 8.000000000000017764 ) ;
#6415 = DIRECTION ( 'NONE',  ( -0.000000000000000000, -0.000000000000000000, 1.000000000000000000 ) ) ;
#6416 = CIRCLE ( 'NONE', #4568, 7.250000000000002665 ) ;
#6417 = ADVANCED_FACE ( 'NONE', ( #2197 ), #7381, .F. ) ;
#6418 = DIRECTION ( 'NONE',  ( -1.000000000000000000, -0.000000000000000000, -0.000000000000000000 ) ) ;
#6419 = ADVANCED_FACE ( 'NONE', ( #7335 ), #757, .F. ) ;
#6420 = DIRECTION ( 'NONE',  ( -1.000000000000000000, 0.000000000000000000, 0.000000000000000000 ) ) ;
#6421 = EDGE_CURVE ( 'NONE', #2884, #794, #1045, .T. ) ;
#6422 = EDGE_CURVE ( 'NONE', #1673, #3807, #5470, .T. ) ;
#6423 = LINE ( 'NONE', #5701, #1127 ) ;
#6424 = ORIENTED_EDGE ( 'NONE', *, *, #3536, .F. ) ;
#6425 = ORIENTED_EDGE ( 'NONE', *, *, #1833, .F. ) ;
#6426 = FACE_OUTER_BOUND ( 'NONE', #6463, .T. ) ;
#6427 = VERTEX_POINT ( 'NONE', #9107 ) ;
#6428 = DIRECTION ( 'NONE',  ( 1.000000000000000000, 0.000000000000000000, 0.000000000000000000 ) ) ;
#6429 = DIRECTION ( 'NONE',  ( 0.000000000000000000, 0.000000000000000000, 1.000000000000000000 ) ) ;
#6430 = VECTOR ( 'NONE', #2142, 1000.000000000000114 ) ;
#6431 = DIRECTION ( 'NONE',  ( 0.000000000000000000, 0.000000000000000000, 1.000000000000000000 ) ) ;
#6432 = AXIS2_PLACEMENT_3D ( 'NONE', #6015, #2931, #2164 ) ;
#6433 = FACE_OUTER_BOUND ( 'NONE', #4818, .T. ) ;
#6434 = B_SPLINE_CURVE_WITH_KNOTS ( 'NONE', 3,
 ( #7694, #9173, #8982, #1780, #5351, #6167, #7645, #1013, #2608, #6837, #5534, #6976, #300, #3948 ),
 .UNSPECIFIED., .F., .F.,
 ( 4, 2, 2, 2, 2, 2, 4 ),
 ( 0.008014353914675855992, 0.01001537843003033959, 0.01101589068770758226, 0.01201640294538482492, 0.01301691520306206759, 0.01401742746073931199, 0.01601845197609379906 ),
 .UNSPECIFIED. ) ;
#6435 = CARTESIAN_POINT ( 'NONE',  ( 16.00000000000000000, 43.00000000000000000, 11.99999999999999645 ) ) ;
#6436 = AXIS2_PLACEMENT_3D ( 'NONE', #1511, #6569, #8863 ) ;
#6437 = CARTESIAN_POINT ( 'NONE',  ( 37.22467645238197775, -47.05659850664388699, -5.608807313787648852 ) ) ;
#6438 = EDGE_CURVE ( 'NONE', #7709, #6770, #5568, .T. ) ;
#6439 = ORIENTED_EDGE ( 'NONE', *, *, #9287, .T. ) ;
#6440 = VECTOR ( 'NONE', #3231, 1000.000000000000114 ) ;
#6441 = VERTEX_POINT ( 'NONE', #8492 ) ;
#6442 = DIRECTION ( 'NONE',  ( 0.5773502691896281735, 0.000000000000000000, -0.8164965809277242581 ) ) ;
#6443 = CONTEXT_DEPENDENT_SHAPE_REPRESENTATION ( #2155, #8078 ) ;
#6444 = ADVANCED_FACE ( 'NONE', ( #8395 ), #4415, .F. ) ;
#6445 = CARTESIAN_POINT ( 'NONE',  ( 0.000000000000000000, 0.000000000000000000, 1.000000000000000000 ) ) ;
#6446 = CARTESIAN_POINT ( 'NONE',  ( 3.499999999999999556, 0.000000000000000000, 22.50000000000000000 ) ) ;
#6447 = LINE ( 'NONE', #9362, #1895 ) ;
#6448 = PLANE ( 'NONE',  #9008 ) ;
#6449 = EDGE_LOOP ( 'NONE', ( #5520, #353, #537, #5366 ) ) ;
#6450 = ORIENTED_EDGE ( 'NONE', *, *, #194, .F. ) ;
#6451 = EDGE_LOOP ( 'NONE', ( #264, #4045, #7939, #2194 ) ) ;
#6452 = AXIS2_PLACEMENT_3D ( 'NONE', #9371, #4907, #2798 ) ;
#6453 = EDGE_LOOP ( 'NONE', ( #7811, #3623, #9136, #1714 ) ) ;
#6454 = DIRECTION ( 'NONE',  ( -0.000000000000000000, -0.000000000000000000, -1.000000000000000000 ) ) ;
#6455 = FACE_OUTER_BOUND ( 'NONE', #1700, .T. ) ;
#6456 = DIRECTION ( 'NONE',  ( -0.000000000000000000, -0.000000000000000000, -1.000000000000000000 ) ) ;
#6457 = CYLINDRICAL_SURFACE ( 'NONE', #3552, 12.50000000000000000 ) ;
#6458 = EDGE_CURVE ( 'NONE', #3040, #5577, #431, .T. ) ;
#6459 = DIRECTION ( 'NONE',  ( 0.000000000000000000, 0.000000000000000000, -1.000000000000000000 ) ) ;
#6460 = CONICAL_SURFACE ( 'NONE', #3079, 30.00000000000000000, 0.7853981633974428389 ) ;
#6461 = ORIENTED_EDGE ( 'NONE', *, *, #7768, .F. ) ;
#6462 = LINE ( 'NONE', #776, #8693 ) ;
#6463 = EDGE_LOOP ( 'NONE', ( #6539, #8600 ) ) ;
#6464 = DIRECTION ( 'NONE',  ( 0.000000000000000000, 0.000000000000000000, -1.000000000000000000 ) ) ;
#6465 = EDGE_CURVE ( 'NONE', #3685, #4695, #9318, .T. ) ;
#6466 = CARTESIAN_POINT ( 'NONE',  ( 50.79490495164537833, 29.99999999999999645, -82.50000000000000000 ) ) ;
#6467 = VECTOR ( 'NONE', #9440, 1000.000000000000114 ) ;
#6468 = LINE ( 'NONE', #497, #4161 ) ;
#6469 = DIRECTION ( 'NONE',  ( 0.000000000000000000, 1.000000000000000000, -0.000000000000000000 ) ) ;
#6470 = DIRECTION ( 'NONE',  ( -0.000000000000000000, -0.000000000000000000, -1.000000000000000000 ) ) ;
#6471 = ORIENTED_EDGE ( 'NONE', *, *, #4209, .F. ) ;
#6472 = ORIENTED_EDGE ( 'NONE', *, *, #2807, .T. ) ;
#6473 = CARTESIAN_POINT ( 'NONE',  ( 0.000000000000000000, 7.653668647300657213, -17.72759065022447089 ) ) ;
#6474 = ORIENTED_EDGE ( 'NONE', *, *, #5213, .T. ) ;
#6475 = LINE ( 'NONE', #1267, #5669 ) ;
#6476 = CARTESIAN_POINT ( 'NONE',  ( 19.00000000000000000, 0.000000000000000000, 0.000000000000000000 ) ) ;
#6477 = DIRECTION ( 'NONE',  ( 1.000000000000000000, 0.000000000000000000, 0.000000000000000000 ) ) ;
#6478 = AXIS2_PLACEMENT_3D ( 'NONE', #2278, #2428, #5359 ) ;
#6479 = DIRECTION ( 'NONE',  ( -0.000000000000000000, -0.000000000000000000, -1.000000000000000000 ) ) ;
#6480 = EDGE_CURVE ( 'NONE', #5908, #8953, #6867, .T. ) ;
#6481 = DIRECTION ( 'NONE',  ( -0.5773502691896235106, -0.000000000000000000, 0.8164965809277276998 ) ) ;
#6482 = CARTESIAN_POINT ( 'NONE',  ( 2.265596578422603791E-15, 35.00000000000000000, 13.49999999999999822 ) ) ;
#6483 = EDGE_CURVE ( 'NONE', #458, #1974, #3806, .T. ) ;
#6484 = ORIENTED_EDGE ( 'NONE', *, *, #6128, .F. ) ;
#6485 = EDGE_LOOP ( 'NONE', ( #3967, #8493, #5049, #4270 ) ) ;
#6486 = COLOUR_RGB ( '',0.7921568627450980005, 0.8196078431372548767, 0.9333333333333333481 ) ;
#6487 = DIRECTION ( 'NONE',  ( 0.000000000000000000, 0.000000000000000000, -1.000000000000000000 ) ) ;
#6488 = ORIENTED_EDGE ( 'NONE', *, *, #3400, .F. ) ;
#6489 = CIRCLE ( 'NONE', #7865, 11.00000000000000000 ) ;
#6490 = DIRECTION ( 'NONE',  ( 0.000000000000000000, 0.000000000000000000, 1.000000000000000000 ) ) ;
#6491 = CARTESIAN_POINT ( 'NONE',  ( 0.000000000000000000, 0.000000000000000000, 21.00000000000000000 ) ) ;
#6492 = DIRECTION ( 'NONE',  ( 0.000000000000000000, 0.000000000000000000, 1.000000000000000000 ) ) ;
#6493 = ORIENTED_EDGE ( 'NONE', *, *, #6168, .T. ) ;
#6494 = VERTEX_POINT ( 'NONE', #6958 ) ;
#6495 = AXIS2_PLACEMENT_3D ( 'NONE', #5695, #5012, #8570 ) ;
#6496 = ORIENTED_EDGE ( 'NONE', *, *, #6128, .T. ) ;
#6497 = EDGE_LOOP ( 'NONE', ( #3284, #8872, #1424, #834 ) ) ;
#6498 = CARTESIAN_POINT ( 'NONE',  ( 27.81257783158193675, -2.818165554823583552, 0.9523463990989768924 ) ) ;
#6499 = DIRECTION ( 'NONE',  ( 0.000000000000000000, 0.000000000000000000, -1.000000000000000000 ) ) ;
#6500 = FACE_OUTER_BOUND ( 'NONE', #2724, .T. ) ;
#6501 = VECTOR ( 'NONE', #2320, 1000.000000000000114 ) ;
#6502 = CARTESIAN_POINT ( 'NONE',  ( -28.66635145370234383, -1.351859493328359196, 1.696225934522937351 ) ) ;
#6503 = PLANE ( 'NONE',  #273 ) ;
#6504 = ORIENTED_EDGE ( 'NONE', *, *, #4714, .T. ) ;
#6505 = ORIENTED_EDGE ( 'NONE', *, *, #145, .T. ) ;
#6506 = CARTESIAN_POINT ( 'NONE',  ( 16.00000000000000000, 43.00000000000000000, -7.366666666666667140 ) ) ;
#6507 = CIRCLE ( 'NONE', #3277, 12.50000000000000000 ) ;
#6508 = CARTESIAN_POINT ( 'NONE',  ( -28.06144414093873962, 2.260912237343719600, 1.151721138160513469 ) ) ;
#6509 = CARTESIAN_POINT ( 'NONE',  ( -50.79490495164537833, -12.50000000000000000, -100.0000000000000000 ) ) ;
#6510 = CARTESIAN_POINT ( 'NONE',  ( 19.00000000000000000, 0.000000000000000000, 0.000000000000000000 ) ) ;
#6511 = EDGE_CURVE ( 'NONE', #7510, #4010, #9152, .T. ) ;
#6512 = CARTESIAN_POINT ( 'NONE',  ( 22.50000000000000355, 0.000000000000000000, 10.00000000000000000 ) ) ;
#6513 = VERTEX_POINT ( 'NONE', #2589 ) ;
#6514 = ORIENTED_EDGE ( 'NONE', *, *, #4953, .T. ) ;
#6515 = VERTEX_POINT ( 'NONE', #7577 ) ;
#6516 = CARTESIAN_POINT ( 'NONE',  ( -27.16400976452049321, -3.794195651236124789, 0.4256031388450376984 ) ) ;
#6517 = AXIS2_PLACEMENT_3D ( 'NONE', #1519, #1304, #4454 ) ;
#6518 = CARTESIAN_POINT ( 'NONE',  ( 60.00000000000000000, 15.90990257669733943, -51.09009742330271564 ) ) ;
#6519 = LINE ( 'NONE', #7276, #7149 ) ;
#6520 = AXIS2_PLACEMENT_3D ( 'NONE', #7738, #432, #1196 ) ;
#6521 = CARTESIAN_POINT ( 'NONE',  ( -26.99999999999998934, -34.99999999999999289, 58.99999999999997158 ) ) ;
#6522 = EDGE_CURVE ( 'NONE', #1857, #777, #3492, .T. ) ;
#6523 = CARTESIAN_POINT ( 'NONE',  ( 4.000000000000000000, 18.47759065022658120, 7.653668647302884764 ) ) ;
#6524 = CARTESIAN_POINT ( 'NONE',  ( 4.000000000000000000, 0.000000000000000000, 22.00000000000000355 ) ) ;
#6525 = VERTEX_POINT ( 'NONE', #1135 ) ;
#6526 = ORIENTED_EDGE ( 'NONE', *, *, #1111, .F. ) ;
#6527 = DIRECTION ( 'NONE',  ( 0.000000000000000000, 0.000000000000000000, -1.000000000000000000 ) ) ;
#6528 = AXIS2_PLACEMENT_3D ( 'NONE', #3386, #409, #1175 ) ;
#6529 = DIRECTION ( 'NONE',  ( 1.000000000000000000, 0.000000000000000000, 0.000000000000000000 ) ) ;
#6530 = EDGE_CURVE ( 'NONE', #3262, #3430, #7001, .T. ) ;
#6531 = EDGE_CURVE ( 'NONE', #7382, #5267, #3348, .T. ) ;
#6532 = CARTESIAN_POINT ( 'NONE',  ( 37.99999999999999289, -44.39318849903271769, -6.762951650419152472 ) ) ;
#6533 = ADVANCED_FACE ( 'NONE', ( #2089 ), #7135, .T. ) ;
#6534 = EDGE_CURVE ( 'NONE', #1974, #3407, #653, .T. ) ;
#6535 = DIRECTION ( 'NONE',  ( -1.000000000000000000, -0.000000000000000000, -0.000000000000000000 ) ) ;
#6536 = DIRECTION ( 'NONE',  ( 0.000000000000000000, 0.000000000000000000, -1.000000000000000000 ) ) ;
#6537 = ORIENTED_EDGE ( 'NONE', *, *, #2885, .T. ) ;
#6538 = VERTEX_POINT ( 'NONE', #7904 ) ;
#6539 = ORIENTED_EDGE ( 'NONE', *, *, #2328, .T. ) ;
#6540 = ORIENTED_EDGE ( 'NONE', *, *, #2944, .F. ) ;
#6541 = CARTESIAN_POINT ( 'NONE',  ( -13.50000000000000178, 1.653273178848927064E-15, 27.50000000000000355 ) ) ;
#6542 = LINE ( 'NONE', #7394, #2578 ) ;
#6543 = CIRCLE ( 'NONE', #7143, 3.000000000000002665 ) ;
#6544 = DIRECTION ( 'NONE',  ( -0.000000000000000000, -0.000000000000000000, 1.000000000000000000 ) ) ;
#6545 = EDGE_CURVE ( 'NONE', #6084, #3451, #5039, .T. ) ;
#6546 = CARTESIAN_POINT ( 'NONE',  ( -15.99999999999999645, 49.08300322764473123, -4.730698601353950039 ) ) ;
#6547 = EDGE_CURVE ( 'NONE', #3622, #2677, #555, .T. ) ;
#6548 = CARTESIAN_POINT ( 'NONE',  ( 16.50000000000000000, 0.000000000000000000, 2.000000000000035083 ) ) ;
#6549 = DIRECTION ( 'NONE',  ( 0.000000000000000000, 0.000000000000000000, 1.000000000000000000 ) ) ;
#6550 = EDGE_CURVE ( 'NONE', #777, #1857, #4272, .T. ) ;
#6551 = ORIENTED_EDGE ( 'NONE', *, *, #2603, .F. ) ;
#6552 = AXIS2_PLACEMENT_3D ( 'NONE', #271, #454, #3469 ) ;
#6553 = CIRCLE ( 'NONE', #8212, 6.000000000000000000 ) ;
#6554 = DIRECTION ( 'NONE',  ( -0.000000000000000000, -0.000000000000000000, -1.000000000000000000 ) ) ;
#6555 = ORIENTED_EDGE ( 'NONE', *, *, #3550, .F. ) ;
#6556 = CYLINDRICAL_SURFACE ( 'NONE', #1410, 15.00000000000000000 ) ;
#6557 = CARTESIAN_POINT ( 'NONE',  ( 0.000000000000000000, -22.50000000000000355, 10.00000000000000000 ) ) ;
#6558 = DIRECTION ( 'NONE',  ( 0.5773502691896291728, -0.000000000000000000, 0.8164965809277235920 ) ) ;
#6559 = AXIS2_PLACEMENT_3D ( 'NONE', #113, #6752, #8896 ) ;
#6560 = FACE_OUTER_BOUND ( 'NONE', #4193, .T. ) ;
#6561 = AXIS2_PLACEMENT_3D ( 'NONE', #3462, #9271, #6459 ) ;
#6562 = CARTESIAN_POINT ( 'NONE',  ( -4.077745023575802819, -26.91684391854058589, 0.2223699321171553334 ) ) ;
#6563 = ORIENTED_EDGE ( 'NONE', *, *, #2522, .T. ) ;
#6564 = ORIENTED_EDGE ( 'NONE', *, *, #6220, .F. ) ;
#6565 = FILL_AREA_STYLE ('',( #5265 ) ) ;
#6566 = MECHANICAL_DESIGN_GEOMETRIC_PRESENTATION_REPRESENTATION (  '', ( #8089 ), #2726 ) ;
#6567 = EDGE_LOOP ( 'NONE', ( #7193, #9214, #845, #2084 ) ) ;
#6568 = AXIS2_PLACEMENT_3D ( 'NONE', #3125, #2410, #8932 ) ;
#6569 = DIRECTION ( 'NONE',  ( -1.000000000000000000, 0.000000000000000000, 0.000000000000000000 ) ) ;
#6570 = CARTESIAN_POINT ( 'NONE',  ( -26.99999999999998934, -34.99999999999999289, 58.99999999999997158 ) ) ;
#6571 = CARTESIAN_POINT ( 'NONE',  ( -5.999999999999842792, -22.50000000000000355, 5.000000000000000000 ) ) ;
#6572 = VECTOR ( 'NONE', #1962, 1000.000000000000000 ) ;
#6573 = DIRECTION ( 'NONE',  ( -0.000000000000000000, -0.000000000000000000, 1.000000000000000000 ) ) ;
#6574 = LINE ( 'NONE', #8819, #5602 ) ;
#6575 = CARTESIAN_POINT ( 'NONE',  ( 19.00000000000000000, 0.000000000000000000, 0.000000000000000000 ) ) ;
#6576 = EDGE_CURVE ( 'NONE', #8983, #5672, #3039, .T. ) ;
#6577 = EDGE_LOOP ( 'NONE', ( #8915, #7552 ) ) ;
#6578 = ORIENTED_EDGE ( 'NONE', *, *, #713, .T. ) ;
#6579=STYLED_ITEM('',(#9515),#6348);
#6580 = FACE_OUTER_BOUND ( 'NONE', #2149, .T. ) ;
#6581 = CARTESIAN_POINT ( 'NONE',  ( -27.00000000000000000, 43.00000000000000000, 11.99999999999999645 ) ) ;
#6582 = AXIS2_PLACEMENT_3D ( 'NONE', #2338, #8905, #2909 ) ;
#6583 = AXIS2_PLACEMENT_3D ( 'NONE', #2222, #5106, #1653 ) ;
#6584 = CARTESIAN_POINT ( 'NONE',  ( 37.22467645238197775, -47.05659850664388699, -5.608807313787648852 ) ) ;
#6585 = APPLICATION_CONTEXT ( 'automotive_design' ) ;
#6586 = DIRECTION ( 'NONE',  ( -1.000000000000000000, 0.000000000000000000, 0.000000000000000000 ) ) ;
#6587 = VERTEX_POINT ( 'NONE', #4307 ) ;
#6588 = ORIENTED_EDGE ( 'NONE', *, *, #2191, .T. ) ;
#6589 = EDGE_LOOP ( 'NONE', ( #8970, #4328, #2644, #9114 ) ) ;
#6590 = CARTESIAN_POINT ( 'NONE',  ( 70.51394605043111596, 64.54333883338001954, 28.04625972168100390 ) ) ;
#6591 = VECTOR ( 'NONE', #2268, 1000.000000000000000 ) ;
#6592 = ORIENTED_EDGE ( 'NONE', *, *, #6438, .F. ) ;
#6593 = EDGE_CURVE ( 'NONE', #5576, #2697, #5501, .T. ) ;
#6594 = CARTESIAN_POINT ( 'NONE',  ( -15.99999999999999645, 43.00000000000000000, -7.366666666666667140 ) ) ;
#6595 = EDGE_CURVE ( 'NONE', #3451, #2056, #9245, .T. ) ;
#6596 = LINE ( 'NONE', #5867, #9470 ) ;
#6597 = CARTESIAN_POINT ( 'NONE',  ( 0.000000000000000000, 0.000000000000000000, 21.00000000000000000 ) ) ;
#6598 = PLANE ( 'NONE',  #2025 ) ;
#6599 = DIRECTION ( 'NONE',  ( 0.000000000000000000, 0.7071067811865479058, -0.7071067811865472397 ) ) ;
#6600 = DIRECTION ( 'NONE',  ( 0.000000000000000000, 0.000000000000000000, -1.000000000000000000 ) ) ;
#6601 =( BOUNDED_CURVE ( )  B_SPLINE_CURVE ( 3, ( #4570, #7546, #1635, #8355 ),
 .UNSPECIFIED., .F., .T. ) 
 B_SPLINE_CURVE_WITH_KNOTS ( ( 4, 4 ),
 ( 0.6692669939101993926, 1.047197551196597853 ),
 .UNSPECIFIED. ) 
 CURVE ( )  GEOMETRIC_REPRESENTATION_ITEM ( )  RATIONAL_B_SPLINE_CURVE ( ( 1.000000000000000000, 0.9881327504826167285, 0.9881327504826167285, 1.000000000000000000 ) ) 
 REPRESENTATION_ITEM ( '' )  );
#6602 = EDGE_CURVE ( 'NONE', #6513, #1435, #893, .T. ) ;
#6603 = EDGE_LOOP ( 'NONE', ( #1387, #7953 ) ) ;
#6604 = DIRECTION ( 'NONE',  ( -1.000000000000000000, -0.000000000000000000, -0.000000000000000000 ) ) ;
#6605 = ORIENTED_EDGE ( 'NONE', *, *, #5711, .F. ) ;
#6606 = CARTESIAN_POINT ( 'NONE',  ( -26.99999999999998934, -34.99999999999999289, 64.00000000000000000 ) ) ;
#6607 = DIRECTION ( 'NONE',  ( 0.000000000000000000, 0.000000000000000000, 1.000000000000000000 ) ) ;
#6608 = CARTESIAN_POINT ( 'NONE',  ( 8.000000000000021316, -22.50000000000000355, 0.000000000000000000 ) ) ;
#6609 = CARTESIAN_POINT ( 'NONE',  ( -22.50000000000000355, 0.000000000000000000, 0.000000000000000000 ) ) ;
#6610 = ORIENTED_EDGE ( 'NONE', *, *, #2522, .F. ) ;
#6611 = VERTEX_POINT ( 'NONE', #5707 ) ;
#6612 = CARTESIAN_POINT ( 'NONE',  ( 3.157268078127849265, 27.61694991999677029, 0.7947205175373169839 ) ) ;
#6613 = VERTEX_POINT ( 'NONE', #507 ) ;
#6614 = CARTESIAN_POINT ( 'NONE',  ( 0.4999999999999935052, 0.000000000000000000, 0.000000000000000000 ) ) ;
#6615 = DIRECTION ( 'NONE',  ( 0.000000000000000000, 0.000000000000000000, -1.000000000000000000 ) ) ;
#6616 = AXIS2_PLACEMENT_3D ( 'NONE', #7092, #8729, #8627 ) ;
#6617 = DIRECTION ( 'NONE',  ( 1.000000000000000000, 0.000000000000000000, 0.000000000000000000 ) ) ;
#6618 = DIRECTION ( 'NONE',  ( 0.000000000000000000, 0.000000000000000000, 1.000000000000000000 ) ) ;
#6619 = CARTESIAN_POINT ( 'NONE',  ( 0.000000000000000000, -34.99999999999999289, 13.50000000000001243 ) ) ;
#6620 = CARTESIAN_POINT ( 'NONE',  ( 37.00000000000000000, -15.90990257669733943, -85.90990257669729147 ) ) ;
#6621 = CYLINDRICAL_SURFACE ( 'NONE', #669, 13.66147716702868031 ) ;
#6622 = EDGE_LOOP ( 'NONE', ( #4985, #4485 ) ) ;
#6623 = ORIENTED_EDGE ( 'NONE', *, *, #5675, .F. ) ;
#6624 = CARTESIAN_POINT ( 'NONE',  ( 22.50000000000000355, 0.000000000000000000, 0.000000000000000000 ) ) ;
#6625 = PRODUCT_DEFINITION_SHAPE ( 'NONE', 'NONE',  #9497 ) ;
#6626 = CARTESIAN_POINT ( 'NONE',  ( -2.663458823497500294, 28.40635703822599822, 1.529086667430999524 ) ) ;
#6627 = EDGE_CURVE ( 'NONE', #7881, #8797, #9392, .T. ) ;
#6628 = CYLINDRICAL_SURFACE ( 'NONE', #70, 1.560000000002327303 ) ;
#6629 = FACE_OUTER_BOUND ( 'NONE', #355, .T. ) ;
#6630 = CIRCLE ( 'NONE', #7699, 8.000000000000021316 ) ;
#6631 = VERTEX_POINT ( 'NONE', #7228 ) ;
#6632 = ADVANCED_FACE ( 'NONE', ( #4974 ), #3435, .F. ) ;
#6633 = ORIENTED_EDGE ( 'NONE', *, *, #4475, .F. ) ;
#6634 = VERTEX_POINT ( 'NONE', #1225 ) ;
#6635 = CARTESIAN_POINT ( 'NONE',  ( 22.66898259762535872, 16.78747270278774906, 29.10812554498839688 ) ) ;
#6636 = ORIENTED_EDGE ( 'NONE', *, *, #9402, .T. ) ;
#6637 = DIRECTION ( 'NONE',  ( -1.000000000000000000, 0.000000000000000000, 0.000000000000000000 ) ) ;
#6638 = FACE_OUTER_BOUND ( 'NONE', #5264, .T. ) ;
#6639 = CARTESIAN_POINT ( 'NONE',  ( -17.50000000000000355, 2.143131898507868643E-15, 14.49999999999999822 ) ) ;
#6640 = CARTESIAN_POINT ( 'NONE',  ( 22.50000000000000355, 0.000000000000000000, 5.000000000000000000 ) ) ;
#6641 = CIRCLE ( 'NONE', #5870, 7.250000000000002665 ) ;
#6642 = DIRECTION ( 'NONE',  ( 0.000000000000000000, 0.000000000000000000, 1.000000000000000000 ) ) ;
#6643 = LINE ( 'NONE', #6687, #873 ) ;
#6644 = ORIENTED_EDGE ( 'NONE', *, *, #9124, .T. ) ;
#6645 = CARTESIAN_POINT ( 'NONE',  ( -15.99999999999999645, -43.00000000000000000, 11.99999999999999645 ) ) ;
#6646 = ORIENTED_EDGE ( 'NONE', *, *, #6305, .F. ) ;
#6647 = DIRECTION ( 'NONE',  ( 0.000000000000000000, 0.000000000000000000, 1.000000000000000000 ) ) ;
#6648 = DIRECTION ( 'NONE',  ( 0.000000000000000000, 0.000000000000000000, -1.000000000000000000 ) ) ;
#6649 = EDGE_CURVE ( 'NONE', #5465, #3092, #4884, .T. ) ;
#6651 = EDGE_CURVE ( 'NONE', #4745, #7535, #1499, .T. ) ;
#6650 = CARTESIAN_POINT ( 'NONE',  ( 0.000000000000000000, 0.000000000000000000, 0.000000000000000000 ) ) ;
#6652 = EDGE_CURVE ( 'NONE', #8082, #6389, #4874, .T. ) ;
#6653 = DIRECTION ( 'NONE',  ( 0.5773502691896271743, 0.000000000000000000, -0.8164965809277250353 ) ) ;
#6654 = EDGE_CURVE ( 'NONE', #7697, #6367, #3974, .T. ) ;
#6655 = ORIENTED_EDGE ( 'NONE', *, *, #950, .F. ) ;
#6656 = VECTOR ( 'NONE', #4899, 999.9999999999998863 ) ;
#6657 = ORIENTED_EDGE ( 'NONE', *, *, #4335, .T. ) ;
#6658 = SURFACE_SIDE_STYLE ('',( #2180 ) ) ;
#6659 = ORIENTED_EDGE ( 'NONE', *, *, #1294, .F. ) ;
#6660 = DIRECTION ( 'NONE',  ( -1.000000000000000000, 0.000000000000000000, 0.000000000000000000 ) ) ;
#6661 = DIRECTION ( 'NONE',  ( -0.000000000000000000, -0.000000000000000000, -1.000000000000000000 ) ) ;
#6662 = LINE ( 'NONE', #5316, #5007 ) ;
#6663 = DIRECTION ( 'NONE',  ( 1.000000000000000000, -0.000000000000000000, -0.000000000000000000 ) ) ;
#6664 = CARTESIAN_POINT ( 'NONE',  ( -53.29490495164537833, -27.56180520566615044, -41.61356529332876875 ) ) ;
#6665 = EDGE_CURVE ( 'NONE', #8519, #3283, #2277, .T. ) ;
#6666 = CARTESIAN_POINT ( 'NONE',  ( -13.50000000000000178, 1.653273178848927064E-15, 28.50000000000000355 ) ) ;
#6667 = DIRECTION ( 'NONE',  ( -0.5773502691896258421, -0.5773502691896225114, -0.5773502691896290617 ) ) ;
#6668 = ORIENTED_EDGE ( 'NONE', *, *, #5881, .T. ) ;
#6669 = AXIS2_PLACEMENT_3D ( 'NONE', #290, #953, #6821 ) ;
#6670 = ORIENTED_EDGE ( 'NONE', *, *, #7626, .T. ) ;
#6671 = EDGE_CURVE ( 'NONE', #3861, #3211, #6889, .T. ) ;
#6672 = FACE_OUTER_BOUND ( 'NONE', #2783, .T. ) ;
#6673 = AXIS2_PLACEMENT_3D ( 'NONE', #4494, #3729, #6806 ) ;
#6674 = EDGE_LOOP ( 'NONE', ( #8137, #1721, #1390, #967, #8822, #4744, #4281 ) ) ;
#6675 = CARTESIAN_POINT ( 'NONE',  ( 4.506465992502256768, 27.73646215562212092, 1.098439957185652682 ) ) ;
#6676 = CARTESIAN_POINT ( 'NONE',  ( 4.000000000000000000, -9.628187502531647418E-13, -18.43999999999823913 ) ) ;
#6677 = CARTESIAN_POINT ( 'NONE',  ( 0.7500000000000000000, 2.749999999999995559, 1.500000000000000000 ) ) ;
#6678 = ORIENTED_EDGE ( 'NONE', *, *, #9231, .F. ) ;
#6679 = ORIENTED_EDGE ( 'NONE', *, *, #3410, .T. ) ;
#6680 =( LENGTH_UNIT ( ) NAMED_UNIT ( * ) SI_UNIT ( .MILLI., .METRE. ) );
#6681 = CYLINDRICAL_SURFACE ( 'NONE', #6390, 6.000000000000001776 ) ;
#6682 = DIRECTION ( 'NONE',  ( 0.000000000000000000, 0.000000000000000000, -1.000000000000000000 ) ) ;
#6683 = DIRECTION ( 'NONE',  ( -1.000000000000000000, 0.000000000000000000, 0.000000000000000000 ) ) ;
#6684 = CARTESIAN_POINT ( 'NONE',  ( 0.000000000000000000, 0.000000000000000000, 0.000000000000000000 ) ) ;
#6685 = FACE_BOUND ( 'NONE', #3758, .T. ) ;
#6686 = CARTESIAN_POINT ( 'NONE',  ( 5.000000000000000000, -9.628187502531647418E-13, -19.99999999999950262 ) ) ;
#6687 = CARTESIAN_POINT ( 'NONE',  ( -31.99999999999999289, 0.000000000000000000, 14.49999999999999467 ) ) ;
#6688 = EDGE_CURVE ( 'NONE', #2599, #4382, #2001, .T. ) ;
#6689 = ORIENTED_EDGE ( 'NONE', *, *, #2846, .F. ) ;
#6690 = LINE ( 'NONE', #6074, #6265 ) ;
#6691 = ORIENTED_EDGE ( 'NONE', *, *, #6832, .F. ) ;
#6692 = AXIS2_PLACEMENT_3D ( 'NONE', #4074, #3891, #9200 ) ;
#6693 = DIRECTION ( 'NONE',  ( -1.000000000000000000, 0.000000000000000000, -0.000000000000000000 ) ) ;
#6694 = CYLINDRICAL_SURFACE ( 'NONE', #6559, 17.50000000000000000 ) ;
#6695 = CARTESIAN_POINT ( 'NONE',  ( 25.50000000000000355, 3.673940397442054445E-16, 10.00000000000000000 ) ) ;
#6696 = CARTESIAN_POINT ( 'NONE',  ( 0.000000000000000000, 22.50000000000000355, 10.00000000000000000 ) ) ;
#6697 = AXIS2_PLACEMENT_3D ( 'NONE', #2388, #6617, #6707 ) ;
#6698 = ORIENTED_EDGE ( 'NONE', *, *, #1393, .F. ) ;
#6699 = PRODUCT ( '2-Bush', '2-Bush', '', ( #294 ) ) ;
#6700 = ORIENTED_EDGE ( 'NONE', *, *, #2255, .T. ) ;
#6701 = ORIENTED_EDGE ( 'NONE', *, *, #1961, .F. ) ;
#6702 = EDGE_LOOP ( 'NONE', ( #6133, #8376, #9456, #3655, #9044 ) ) ;
#6703 = CARTESIAN_POINT ( 'NONE',  ( -31.99999999999999289, 35.00000000000000000, 59.00000000000000000 ) ) ;
#6704 = ADVANCED_FACE ( 'NONE', ( #2910 ), #2184, .F. ) ;
#6705 = DIRECTION ( 'NONE',  ( -1.000000000000000000, 0.000000000000000000, 0.000000000000000000 ) ) ;
#6706 = VECTOR ( 'NONE', #3667, 1000.000000000000000 ) ;
#6707 = DIRECTION ( 'NONE',  ( 0.000000000000000000, 0.000000000000000000, -1.000000000000000000 ) ) ;
#6708 = AXIS2_PLACEMENT_3D ( 'NONE', #6077, #8279, #6892 ) ;
#6709 = EDGE_CURVE ( 'NONE', #720, #3516, #7465, .T. ) ;
#6710 = ADVANCED_FACE ( 'NONE', ( #3821, #6763 ), #8811, .F. ) ;
#6711 = EDGE_CURVE ( 'NONE', #4960, #2537, #2953, .T. ) ;
#6712 =( REPRESENTATION_RELATIONSHIP ('NONE','NONE', #1933, #8501 ) REPRESENTATION_RELATIONSHIP_WITH_TRANSFORMATION ( #3591 )SHAPE_REPRESENTATION_RELATIONSHIP( ) );
#6713 = CARTESIAN_POINT ( 'NONE',  ( 0.000000000000000000, 1.917977788252103204E-15, -15.66147716702868209 ) ) ;
#6714 = VECTOR ( 'NONE', #9422, 1000.000000000000114 ) ;
#6715 = DIRECTION ( 'NONE',  ( 0.000000000000000000, 0.000000000000000000, 1.000000000000000000 ) ) ;
#6716 = AXIS2_PLACEMENT_3D ( 'NONE', #9408, #2748, #4900 ) ;
#6717 = CARTESIAN_POINT ( 'NONE',  ( -6.000000000000000888, -22.50000000000000355, 2.000000000000013767 ) ) ;
#6718 = PRESENTATION_LAYER_ASSIGNMENT (  '', '', ( #8089 ) ) ;
#6719 = CARTESIAN_POINT ( 'NONE',  ( 28.40858913551337750, -2.655051044735458721, 1.530521587115750037 ) ) ;
#6720 = AXIS2_PLACEMENT_3D ( 'NONE', #3371, #8652, #5588 ) ;
#6721 = ORIENTED_EDGE ( 'NONE', *, *, #5159, .T. ) ;
#6722 = VERTEX_POINT ( 'NONE', #3679 ) ;
#6723 = CIRCLE ( 'NONE', #4873, 3.000000000000000000 ) ;
#6724 = EDGE_CURVE ( 'NONE', #6525, #7742, #1504, .T. ) ;
#6725 = ORIENTED_EDGE ( 'NONE', *, *, #1806, .F. ) ;
#6726 = CIRCLE ( 'NONE', #3032, 3.000000000000002665 ) ;
#6727 = CARTESIAN_POINT ( 'NONE',  ( -4.531045531831497719, 27.74104493317181053, 1.101386028467601141 ) ) ;
#6728 = AXIS2_PLACEMENT_3D ( 'NONE', #380, #4083, #3981 ) ;
#6729 = EDGE_CURVE ( 'NONE', #777, #7742, #8002, .T. ) ;
#6730 = CONICAL_SURFACE ( 'NONE', #4885, 6.000000000000001776, 0.7853981633974500554 ) ;
#6731 = FACE_OUTER_BOUND ( 'NONE', #4065, .T. ) ;
#6732 = PRODUCT_DEFINITION_CONTEXT ( 'detailed design', #4617, 'design' ) ;
#6733 = DIRECTION ( 'NONE',  ( 0.000000000000000000, 0.000000000000000000, -1.000000000000000000 ) ) ;
#6734 = ORIENTED_EDGE ( 'NONE', *, *, #1551, .F. ) ;
#6735 = EDGE_LOOP ( 'NONE', ( #7058, #6033, #209, #344 ) ) ;
#6736 = CARTESIAN_POINT ( 'NONE',  ( -9.137893445389812186, 143.3630823859938914, 27.00630703231499297 ) ) ;
#6737 = EDGE_CURVE ( 'NONE', #1115, #1485, #9176, .T. ) ;
#6738 = DIRECTION ( 'NONE',  ( -0.000000000000000000, -0.000000000000000000, -1.000000000000000000 ) ) ;
#6739 = AXIS2_PLACEMENT_3D ( 'NONE', #2339, #5269, #8192 ) ;
#6740 = AXIS2_PLACEMENT_3D ( 'NONE', #2484, #7516, #268 ) ;
#6741 = DIRECTION ( 'NONE',  ( 1.000000000000000000, 0.000000000000000000, 0.000000000000000000 ) ) ;
#6742 = CARTESIAN_POINT ( 'NONE',  ( 5.000000000000000000, -14.14213562373112154, 14.14213562373418220 ) ) ;
#6743 = CARTESIAN_POINT ( 'NONE',  ( 0.000000000000000000, -22.50000000000000355, 5.000000000000000000 ) ) ;
#6744 = LINE ( 'NONE', #7446, #4594 ) ;
#6745 = DIRECTION ( 'NONE',  ( -1.000000000000000000, 0.000000000000000000, 0.000000000000000000 ) ) ;
#6746 = FACE_OUTER_BOUND ( 'NONE', #946, .T. ) ;
#6747 = AXIS2_PLACEMENT_3D ( 'NONE', #2933, #3753, #103 ) ;
#6748 = ORIENTED_EDGE ( 'NONE', *, *, #1905, .T. ) ;
#6749 = DIRECTION ( 'NONE',  ( -0.000000000000000000, -0.000000000000000000, -1.000000000000000000 ) ) ;
#6750 = ORIENTED_EDGE ( 'NONE', *, *, #5865, .T. ) ;
#6751 = LINE ( 'NONE', #3088, #2805 ) ;
#6752 = DIRECTION ( 'NONE',  ( -1.000000000000000000, -0.000000000000000000, -0.000000000000000000 ) ) ;
#6753 = DIRECTION ( 'NONE',  ( 0.000000000000000000, 0.000000000000000000, -1.000000000000000000 ) ) ;
#6754 = EDGE_CURVE ( 'NONE', #301, #5309, #8102, .T. ) ;
#6755 = DIRECTION ( 'NONE',  ( 1.000000000000000000, -0.000000000000000000, -0.000000000000000000 ) ) ;
#6756 = ORIENTED_EDGE ( 'NONE', *, *, #5219, .T. ) ;
#6757 = ORIENTED_EDGE ( 'NONE', *, *, #3003, .T. ) ;
#6758 = EDGE_CURVE ( 'NONE', #1561, #7674, #3725, .T. ) ;
#6759 = ORIENTED_EDGE ( 'NONE', *, *, #4892, .F. ) ;
#6760 = CARTESIAN_POINT ( 'NONE',  ( 0.000000000000000000, 0.000000000000000000, 0.000000000000000000 ) ) ;
#6761 = ORIENTED_EDGE ( 'NONE', *, *, #6777, .F. ) ;
#6762 = CARTESIAN_POINT ( 'NONE',  ( -51.96152422706632734, -30.00000000000000000, -80.85015119857382615 ) ) ;
#6763 = FACE_OUTER_BOUND ( 'NONE', #6388, .T. ) ;
#6764 = CIRCLE ( 'NONE', #6432, 17.50000000000000355 ) ;
#6765 = DIRECTION ( 'NONE',  ( -1.000000000000000000, 0.000000000000000000, 0.000000000000000000 ) ) ;
#6766 = CARTESIAN_POINT ( 'NONE',  ( 60.00000000000000000, 15.90990257669733943, -57.09009742330271564 ) ) ;
#6767 = DIRECTION ( 'NONE',  ( 0.8660254037844399289, 0.000000000000000000, -0.4999999999999977240 ) ) ;
#6768 = CARTESIAN_POINT ( 'NONE',  ( 39.50000000000000000, -14.99999999999999645, -97.50000000000001421 ) ) ;
#6769 = CARTESIAN_POINT ( 'NONE',  ( 1.571166602479410136E-13, -22.50000000000000355, 15.00000000000000000 ) ) ;
#6770 = VERTEX_POINT ( 'NONE', #6570 ) ;
#6771 = EDGE_LOOP ( 'NONE', ( #3146, #8266, #4325, #7673 ) ) ;
#6772 = CONICAL_SURFACE ( 'NONE', #7068, 6.000000000000000888, 0.7853981633974498333 ) ;
#6773 = DIRECTION ( 'NONE',  ( 0.000000000000000000, 0.000000000000000000, -1.000000000000000000 ) ) ;
#6774 = ORIENTED_EDGE ( 'NONE', *, *, #4257, .T. ) ;
#6775 = DIRECTION ( 'NONE',  ( -1.000000000000000000, 0.000000000000000000, 0.000000000000000000 ) ) ;
#6776 = ADVANCED_FACE ( 'NONE', ( #1462 ), #3153, .F. ) ;
#6777 = EDGE_CURVE ( 'NONE', #6239, #1041, #7961, .T. ) ;
#6778 = DIRECTION ( 'NONE',  ( -1.000000000000000000, -0.000000000000000000, -0.000000000000000000 ) ) ;
#6779 = DIRECTION ( 'NONE',  ( 0.000000000000000000, 0.000000000000000000, 1.000000000000000000 ) ) ;
#6780 = ORIENTED_EDGE ( 'NONE', *, *, #2919, .F. ) ;
#6781 = ORIENTED_EDGE ( 'NONE', *, *, #3599, .T. ) ;
#6782 = FACE_OUTER_BOUND ( 'NONE', #5158, .T. ) ;
#6783 = DIRECTION ( 'NONE',  ( 0.000000000000000000, 0.000000000000000000, 1.000000000000000000 ) ) ;
#6784 = VECTOR ( 'NONE', #3324, 1000.000000000000000 ) ;
#6785 = DIRECTION ( 'NONE',  ( 0.000000000000000000, 0.7071067811865473507, 0.7071067811865477948 ) ) ;
#6786 = DIRECTION ( 'NONE',  ( 1.000000000000000000, 0.000000000000000000, 0.000000000000000000 ) ) ;
#6787 = DIRECTION ( 'NONE',  ( 0.000000000000000000, 0.000000000000000000, 1.000000000000000000 ) ) ;
#6788 = CARTESIAN_POINT ( 'NONE',  ( -3.791949971500568228, -27.16611547376998814, 0.4273392542514636294 ) ) ;
#6789 = EDGE_LOOP ( 'NONE', ( #7430, #5562, #4361, #7777 ) ) ;
#6790 =( NAMED_UNIT ( * ) PLANE_ANGLE_UNIT ( ) SI_UNIT ( $, .RADIAN. ) );
#6791 = ORIENTED_EDGE ( 'NONE', *, *, #6724, .F. ) ;
#6792 = VECTOR ( 'NONE', #1061, 1000.000000000000000 ) ;
#6793 = CARTESIAN_POINT ( 'NONE',  ( -0.7500000000000000000, -2.749999999999995559, 0.000000000000000000 ) ) ;
#6794 = CARTESIAN_POINT ( 'NONE',  ( -37.00000000000000000, 30.00000000000000000, -13.00000000000000000 ) ) ;
#6795 = VECTOR ( 'NONE', #5686, 1000.000000000000000 ) ;
#6796 = DIRECTION ( 'NONE',  ( -0.7071067811865501263, 0.000000000000000000, 0.7071067811865450192 ) ) ;
#6797 = CARTESIAN_POINT ( 'NONE',  ( 53.29490495164537833, 15.90990257669733943, -57.09009742330271564 ) ) ;
#6798 = ORIENTED_EDGE ( 'NONE', *, *, #2322, .T. ) ;
#6799 = EDGE_LOOP ( 'NONE', ( #4448, #5125, #9162, #2139 ) ) ;
#6800 = ORIENTED_EDGE ( 'NONE', *, *, #1525, .F. ) ;
#6801 = VECTOR ( 'NONE', #4640, 1000.000000000000000 ) ;
#6802 = ORIENTED_EDGE ( 'NONE', *, *, #483, .T. ) ;
#6803 = FACE_OUTER_BOUND ( 'NONE', #1481, .T. ) ;
#6804 = CARTESIAN_POINT ( 'NONE',  ( -51.96152422706632734, -30.00000000000000000, -80.85015119857382615 ) ) ;
#6805 = FACE_OUTER_BOUND ( 'NONE', #7719, .T. ) ;
#6806 = DIRECTION ( 'NONE',  ( 0.000000000000000000, 0.000000000000000000, 1.000000000000000000 ) ) ;
#6807 = AXIS2_PLACEMENT_3D ( 'NONE', #5581, #7100, #5680 ) ;
#6808 = SURFACE_STYLE_FILL_AREA ( #8198 ) ;
#6809 = DIRECTION ( 'NONE',  ( -1.000000000000000000, 0.000000000000000000, 0.000000000000000000 ) ) ;
#6810 = ORIENTED_EDGE ( 'NONE', *, *, #1848, .T. ) ;
#6811 = ORIENTED_EDGE ( 'NONE', *, *, #5219, .F. ) ;
#6812 = FACE_OUTER_BOUND ( 'NONE', #8099, .T. ) ;
#6813 = ORIENTED_EDGE ( 'NONE', *, *, #7230, .T. ) ;
#6814 = DIRECTION ( 'NONE',  ( 1.000000000000000000, -0.000000000000000000, 0.000000000000000000 ) ) ;
#6815 = CARTESIAN_POINT ( 'NONE',  ( -26.99999999999998934, -34.99999999999999289, 58.99999999999997158 ) ) ;
#6816 = ORIENTED_EDGE ( 'NONE', *, *, #8934, .T. ) ;
#6817 = AXIS2_PLACEMENT_3D ( 'NONE', #899, #6908, #6809 ) ;
#6818 = EDGE_CURVE ( 'NONE', #386, #7815, #1512, .T. ) ;
#6819 = CARTESIAN_POINT ( 'NONE',  ( -2.341162148116626263, 28.48643429264087246, 1.580564902411995210 ) ) ;
#6820 = CIRCLE ( 'NONE', #9255, 6.000000000000000888 ) ;
#6821 = DIRECTION ( 'NONE',  ( 0.000000000000000000, 0.000000000000000000, 1.000000000000000000 ) ) ;
#6822 = CARTESIAN_POINT ( 'NONE',  ( -2.651740589948411664, -28.40946940741335069, 1.531087476194299413 ) ) ;
#6823 = ORIENTED_EDGE ( 'NONE', *, *, #3307, .T. ) ;
#6824 = CIRCLE ( 'NONE', #8969, 2.999999999999999112 ) ;
#6825 = ORIENTED_EDGE ( 'NONE', *, *, #4319, .F. ) ;
#6826 = EDGE_CURVE ( 'NONE', #4035, #1161, #1687, .T. ) ;
#6827 = CIRCLE ( 'NONE', #525, 1.000000000000000888 ) ;
#6828 = DIRECTION ( 'NONE',  ( 0.000000000000000000, 0.000000000000000000, 1.000000000000000000 ) ) ;
#6829 = DIRECTION ( 'NONE',  ( -1.000000000000000000, 0.000000000000000000, 0.000000000000000000 ) ) ;
#6830 = ADVANCED_FACE ( 'NONE', ( #8864 ), #2285, .F. ) ;
#6831 = AXIS2_PLACEMENT_3D ( 'NONE', #8593, #9360, #5580 ) ;
#6832 = EDGE_CURVE ( 'NONE', #4623, #5974, #8873, .T. ) ;
#6833 = EDGE_CURVE ( 'NONE', #8143, #5323, #1351, .T. ) ;
#6834 = LINE ( 'NONE', #962, #3757 ) ;
#6835 = SURFACE_SIDE_STYLE ('',( #4668 ) ) ;
#6836 = DIRECTION ( 'NONE',  ( -0.000000000000000000, -0.000000000000000000, -1.000000000000000000 ) ) ;
#6837 = CARTESIAN_POINT ( 'NONE',  ( -27.44426127775441415, 5.090287965588961683, 0.9105965356992786752 ) ) ;
#6838 = ORIENTED_EDGE ( 'NONE', *, *, #419, .F. ) ;
#6839 = DIRECTION ( 'NONE',  ( 0.000000000000000000, 0.000000000000000000, -1.000000000000000000 ) ) ;
#6840 = VERTEX_POINT ( 'NONE', #1609 ) ;
#6841 = DIRECTION ( 'NONE',  ( -0.7071067811865455743, 0.000000000000000000, -0.7071067811865494601 ) ) ;
#6842 = CARTESIAN_POINT ( 'NONE',  ( 4.000000000000000000, 7.653668647302530381, 19.22759065022631830 ) ) ;
#6843 = EDGE_CURVE ( 'NONE', #3983, #2056, #1971, .T. ) ;
#6844 = CARTESIAN_POINT ( 'NONE',  ( -22.50000000000000355, 0.000000000000000000, 5.000000000000000000 ) ) ;
#6845 = CARTESIAN_POINT ( 'NONE',  ( 5.000000000000000000, 20.00000000000120437, 1.559999999999680531 ) ) ;
#6846 = EDGE_CURVE ( 'NONE', #8186, #4960, #7517, .T. ) ;
#6847 = ORIENTED_EDGE ( 'NONE', *, *, #3341, .T. ) ;
#6848 = ORIENTED_EDGE ( 'NONE', *, *, #6246, .F. ) ;
#6849 = AXIS2_PLACEMENT_3D ( 'NONE', #2205, #97, #808 ) ;
#6850 = VERTEX_POINT ( 'NONE', #1797 ) ;
#6851 = EDGE_LOOP ( 'NONE', ( #1114, #6302, #4089, #4848 ) ) ;
#6852 = DIRECTION ( 'NONE',  ( 1.000000000000000000, 0.000000000000000000, 0.000000000000000000 ) ) ;
#6853 = LINE ( 'NONE', #7666, #8485 ) ;
#6854 =( BOUNDED_CURVE ( )  B_SPLINE_CURVE ( 3, ( #3860, #1505, #1553, #7455 ),
 .UNSPECIFIED., .F., .F. ) 
 B_SPLINE_CURVE_WITH_KNOTS ( ( 4, 4 ),
 ( 5.497787143782137953, 6.283185307179586232 ),
 .UNSPECIFIED. ) 
 CURVE ( )  GEOMETRIC_REPRESENTATION_ITEM ( )  RATIONAL_B_SPLINE_CURVE ( ( 1.000000000000000000, 0.9492530216741911220, 0.9492530216741911220, 1.000000000000000000 ) ) 
 REPRESENTATION_ITEM ( '' )  );
#6855 = PLANE ( 'NONE',  #1784 ) ;
#6856 = CARTESIAN_POINT ( 'NONE',  ( 0.4999999999999935052, 0.000000000000000000, 0.000000000000000000 ) ) ;
#6857 = DIRECTION ( 'NONE',  ( -0.4999999999999977240, 0.000000000000000000, -0.8660254037844399289 ) ) ;
#6858 = LINE ( 'NONE', #9009, #9305 ) ;
#6859 = CARTESIAN_POINT ( 'NONE',  ( 27.73557521625266631, -4.508354841688211323, 1.097869781876721795 ) ) ;
#6860 = VERTEX_POINT ( 'NONE', #5314 ) ;
#6861 = ORIENTED_EDGE ( 'NONE', *, *, #3809, .F. ) ;
#6862 = CARTESIAN_POINT ( 'NONE',  ( -18.50000000000001776, 0.000000000000000000, 0.000000000000000000 ) ) ;
#6863 = CIRCLE ( 'NONE', #1022, 6.000000000000000888 ) ;
#6864 = ORIENTED_EDGE ( 'NONE', *, *, #4777, .F. ) ;
#6865 = CONICAL_SURFACE ( 'NONE', #6552, 17.50000000000000000, 0.7853981633974552734 ) ;
#6866 = CARTESIAN_POINT ( 'NONE',  ( -26.99999999999998934, 35.00000000000000000, 5.000000000000004441 ) ) ;
#6867 = LINE ( 'NONE', #4072, #7641 ) ;
#6868 = VERTEX_POINT ( 'NONE', #222 ) ;
#6869 = CARTESIAN_POINT ( 'NONE',  ( -9.364477336218600456, -62.15368297487813010, 0.9332626224471969323 ) ) ;
#6870 = CIRCLE ( 'NONE', #7318, 1.000000000000000888 ) ;
#6871 = EDGE_CURVE ( 'NONE', #1677, #5682, #1817, .T. ) ;
#6872 = CARTESIAN_POINT ( 'NONE',  ( 37.00000000000000000, 15.90990257669733943, -85.90990257669729147 ) ) ;
#6873 = CARTESIAN_POINT ( 'NONE',  ( 6.186958832529963814, -26.79406326810229189, 0.4926121009229034176 ) ) ;
#6874 = CIRCLE ( 'NONE', #2732, 6.000000000000001776 ) ;
#6875 = ORIENTED_EDGE ( 'NONE', *, *, #5945, .T. ) ;
#6876 = EDGE_LOOP ( 'NONE', ( #5160, #7584, #8404, #9377 ) ) ;
#6877 = AXIS2_PLACEMENT_3D ( 'NONE', #6396, #4804, #5681 ) ;
#6878 = EDGE_CURVE ( 'NONE', #7550, #3092, #8421, .T. ) ;
#6879 = ITEM_DEFINED_TRANSFORMATION ( 'NONE', 'NONE', #8530,  #1614 ) ;
#6880 = AXIS2_PLACEMENT_3D ( 'NONE', #6624, #8918, #2350 ) ;
#6881 = AXIS2_PLACEMENT_3D ( 'NONE', #630, #9223, #3559 ) ;
#6882 = PLANE ( 'NONE',  #7639 ) ;
#6883 = CARTESIAN_POINT ( 'NONE',  ( 4.703319286132083832, 17.49999999999999645, 49.50000000000000000 ) ) ;
#6884 = PRESENTATION_STYLE_ASSIGNMENT (( #7592 ) ) ;
#6885 = CARTESIAN_POINT ( 'NONE',  ( 6.000000000000000888, 22.50000000000000355, 0.000000000000000000 ) ) ;
#6886 = CARTESIAN_POINT ( 'NONE',  ( -19.62310601229374285, 19.62310601229374285, 26.87436867076458569 ) ) ;
#6887 = ORIENTED_EDGE ( 'NONE', *, *, #7826, .F. ) ;
#6888 = FILL_AREA_STYLE_COLOUR ( '', #7163 ) ;
#6889 = CIRCLE ( 'NONE', #5664, 11.00000000000000000 ) ;
#6890 = VERTEX_POINT ( 'NONE', #270 ) ;
#6891 = DIRECTION ( 'NONE',  ( 1.000000000000000000, 0.000000000000000000, 0.000000000000000000 ) ) ;
#6892 = DIRECTION ( 'NONE',  ( 0.000000000000000000, 0.000000000000000000, -1.000000000000000000 ) ) ;
#6893 = DIRECTION ( 'NONE',  ( 0.000000000000000000, 0.000000000000000000, -1.000000000000000000 ) ) ;
#6894 = FACE_OUTER_BOUND ( 'NONE', #1221, .T. ) ;
#6895 = VECTOR ( 'NONE', #4449, 1000.000000000000000 ) ;
#6896 = EDGE_CURVE ( 'NONE', #4010, #3807, #1750, .T. ) ;
#6897 = VECTOR ( 'NONE', #8141, 1000.000000000000000 ) ;
#6898 = ORIENTED_EDGE ( 'NONE', *, *, #8993, .F. ) ;
#6899 = EDGE_LOOP ( 'NONE', ( #9315, #8110, #6875, #7 ) ) ;
#6900 = EDGE_LOOP ( 'NONE', ( #2587, #8546, #870, #8894 ) ) ;
#6901 =( LENGTH_UNIT ( ) NAMED_UNIT ( * ) SI_UNIT ( .MILLI., .METRE. ) );
#6902 = ORIENTED_EDGE ( 'NONE', *, *, #4168, .F. ) ;
#6903 = DIRECTION ( 'NONE',  ( -0.000000000000000000, -0.000000000000000000, 1.000000000000000000 ) ) ;
#6904 = PLANE ( 'NONE',  #5578 ) ;
#6905 = CARTESIAN_POINT ( 'NONE',  ( 0.000000000000000000, -14.14213562373248401, -14.14213562372942157 ) ) ;
#6906 = DIRECTION ( 'NONE',  ( 1.000000000000000000, 0.000000000000000000, 0.000000000000000000 ) ) ;
#6907 = CARTESIAN_POINT ( 'NONE',  ( 28.48867854402453759, 0.4256064988644707725, 1.491066224433653442 ) ) ;
#6908 = DIRECTION ( 'NONE',  ( -0.000000000000000000, -0.000000000000000000, -1.000000000000000000 ) ) ;
#6909 = EDGE_LOOP ( 'NONE', ( #3076, #8974 ) ) ;
#6910 = ORIENTED_EDGE ( 'NONE', *, *, #4009, .T. ) ;
#6911 = CARTESIAN_POINT ( 'NONE',  ( -26.64999999999998792, 4.333301281932682159, 0.000000000000000000 ) ) ;
#6912 = VERTEX_POINT ( 'NONE', #3971 ) ;
#6913 = DIRECTION ( 'NONE',  ( 0.000000000000000000, 0.000000000000000000, 1.000000000000000000 ) ) ;
#6914 = DIRECTION ( 'NONE',  ( -0.000000000000000000, 1.000000000000000000, -0.000000000000000000 ) ) ;
#6915 = VERTEX_POINT ( 'NONE', #5506 ) ;
#6916 = FACE_OUTER_BOUND ( 'NONE', #9146, .T. ) ;
#6917 = CARTESIAN_POINT ( 'NONE',  ( 0.000000000000000000, -22.50000000000000355, 5.000000000000000000 ) ) ;
#6918 = CYLINDRICAL_SURFACE ( 'NONE', #1651, 30.00000000000000000 ) ;
#6919 = ORIENTED_EDGE ( 'NONE', *, *, #9345, .F. ) ;
#6920 = ORIENTED_EDGE ( 'NONE', *, *, #9419, .F. ) ;
#6921 = ADVANCED_FACE ( 'NONE', ( #8957 ), #6904, .T. ) ;
#6922 = AXIS2_PLACEMENT_3D ( 'NONE', #6230, #402, #272 ) ;
#6923 = DIRECTION ( 'NONE',  ( 0.000000000000000000, -0.7071067811865479058, 0.7071067811865472397 ) ) ;
#6924 = EDGE_CURVE ( 'NONE', #1076, #6279, #2439, .T. ) ;
#6925 = DIRECTION ( 'NONE',  ( -0.000000000000000000, -0.7071067811865455743, -0.7071067811865494601 ) ) ;
#6926 = EDGE_CURVE ( 'NONE', #5995, #1738, #6942, .T. ) ;
#6927 = FILL_AREA_STYLE_COLOUR ( '', #7798 ) ;
#6928 = CARTESIAN_POINT ( 'NONE',  ( -17.50000000000000355, 2.143131898507868643E-15, 63.00000000000002842 ) ) ;
#6929 = CARTESIAN_POINT ( 'NONE',  ( -34.25000000000000000, 43.00000000000000000, -25.00000000000000000 ) ) ;
#6930 = ORIENTED_EDGE ( 'NONE', *, *, #2249, .F. ) ;
#6931 = DIRECTION ( 'NONE',  ( 0.000000000000000000, 0.7071067811865473507, 0.7071067811865477948 ) ) ;
#6932 = VERTEX_POINT ( 'NONE', #8287 ) ;
#6933 = LINE ( 'NONE', #2473, #48 ) ;
#6934 = DIRECTION ( 'NONE',  ( 0.000000000000000000, 0.000000000000000000, 1.000000000000000000 ) ) ;
#6935 = ADVANCED_FACE ( 'NONE', ( #5457 ), #4737, .F. ) ;
#6936 = FACE_OUTER_BOUND ( 'NONE', #7634, .T. ) ;
#6937 = LINE ( 'NONE', #7703, #6179 ) ;
#6938 = AXIS2_PLACEMENT_3D ( 'NONE', #5145, #8839, #3081 ) ;
#6939 = EDGE_LOOP ( 'NONE', ( #2853, #514, #1580, #8805 ) ) ;
#6940 = ORIENTED_EDGE ( 'NONE', *, *, #3044, .F. ) ;
#6941 = EDGE_LOOP ( 'NONE', ( #8010, #7540, #146, #1793 ) ) ;
#6942 = LINE ( 'NONE', #4593, #3114 ) ;
#6943 = EDGE_CURVE ( 'NONE', #8301, #6611, #9238, .T. ) ;
#6944 = CARTESIAN_POINT ( 'NONE',  ( 1.571166602479410136E-13, -22.50000000000000355, 10.00000000000000000 ) ) ;
#6945 = EDGE_CURVE ( 'NONE', #4995, #5110, #2353, .T. ) ;
#6946 = CARTESIAN_POINT ( 'NONE',  ( 12.50000000000000000, 1.530808498934191127E-15, 48.00000000000036948 ) ) ;
#6947 = EDGE_CURVE ( 'NONE', #1286, #233, #3915, .T. ) ;
#6948 = DIRECTION ( 'NONE',  ( 0.000000000000000000, 0.000000000000000000, 1.000000000000000000 ) ) ;
#6949 = EDGE_CURVE ( 'NONE', #1890, #2562, #9217, .T. ) ;
#6950 = EDGE_CURVE ( 'NONE', #662, #7685, #500, .T. ) ;
#6951 = AXIS2_PLACEMENT_3D ( 'NONE', #7506, #7653, #167 ) ;
#6952 = CARTESIAN_POINT ( 'NONE',  ( 2.749999999999996447, -0.7500000000000000000, 1.500000000000000000 ) ) ;
#6953 = ORIENTED_EDGE ( 'NONE', *, *, #8815, .F. ) ;
#6954 = EDGE_LOOP ( 'NONE', ( #186, #265, #5931, #7686 ) ) ;
#6955 = DIRECTION ( 'NONE',  ( 0.000000000000000000, 0.000000000000000000, -1.000000000000000000 ) ) ;
#6956 = EDGE_LOOP ( 'NONE', ( #1783, #9163, #7560, #7824, #3863 ) ) ;
#6957 = DIRECTION ( 'NONE',  ( 0.000000000000000000, 0.000000000000000000, -1.000000000000000000 ) ) ;
#6958 = CARTESIAN_POINT ( 'NONE',  ( 4.000000000000000000, 18.47759065022580316, -6.903668647301629768 ) ) ;
#6959 = EDGE_LOOP ( 'NONE', ( #8315, #3135, #2524, #5785 ) ) ;
#6960 = DIRECTION ( 'NONE',  ( -1.000000000000000000, 0.000000000000000000, 0.000000000000000000 ) ) ;
#6961 = EDGE_CURVE ( 'NONE', #4881, #8783, #6853, .T. ) ;
#6962 = AXIS2_PLACEMENT_3D ( 'NONE', #9306, #4942, #7875 ) ;
#6963 = EDGE_CURVE ( 'NONE', #5505, #5921, #1077, .T. ) ;
#6964 = SHAPE_REPRESENTATION ( '5-Cover', ( #1614 ), #3782 ) ;
#6965 = DIRECTION ( 'NONE',  ( 0.000000000000000000, 0.000000000000000000, 1.000000000000000000 ) ) ;
#6966 = CARTESIAN_POINT ( 'NONE',  ( 27.00000000000000355, -34.99999999999999289, 58.99999999999997158 ) ) ;
#6967 = ADVANCED_FACE ( 'NONE', ( #2526 ), #4782, .F. ) ;
#6968 = ORIENTED_EDGE ( 'NONE', *, *, #1095, .T. ) ;
#6969 = ORIENTED_EDGE ( 'NONE', *, *, #6004, .F. ) ;
#6970 = AXIS2_PLACEMENT_3D ( 'NONE', #9283, #3473, #6328 ) ;
#6971 = ITEM_DEFINED_TRANSFORMATION ( 'NONE', 'NONE', #2702,  #1614 ) ;
#6972 = CARTESIAN_POINT ( 'NONE',  ( -2.499999999999998668, 0.000000000000000000, 21.00000000000000000 ) ) ;
#6973 = DIRECTION ( 'NONE',  ( 0.000000000000000000, 0.000000000000000000, -1.000000000000000000 ) ) ;
#6974 = LINE ( 'NONE', #8271, #6792 ) ;
#6975 = DIRECTION ( 'NONE',  ( -1.000000000000000000, 0.000000000000000000, 0.000000000000000000 ) ) ;
#6976 = CARTESIAN_POINT ( 'NONE',  ( -26.78965207131482984, 6.193975265304562328, 0.4897763315595443090 ) ) ;
#6977 = ORIENTED_EDGE ( 'NONE', *, *, #6924, .T. ) ;
#6978 = CIRCLE ( 'NONE', #2207, 3.000000000000002665 ) ;
#6979 = LINE ( 'NONE', #565, #1186 ) ;
#6980 = ORIENTED_EDGE ( 'NONE', *, *, #9221, .F. ) ;
#6981 = DIRECTION ( 'NONE',  ( 1.000000000000000000, 0.000000000000000000, 0.000000000000000000 ) ) ;
#6982 = CIRCLE ( 'NONE', #4827, 14.49999999999998401 ) ;
#6983 = FACE_OUTER_BOUND ( 'NONE', #4672, .T. ) ;
#6984 = CYLINDRICAL_SURFACE ( 'NONE', #3059, 6.000000000000001776 ) ;
#6985 = DIRECTION ( 'NONE',  ( 0.000000000000000000, 0.000000000000000000, 1.000000000000000000 ) ) ;
#6986 = ORIENTED_EDGE ( 'NONE', *, *, #7911, .F. ) ;
#6987 = ORIENTED_EDGE ( 'NONE', *, *, #1536, .F. ) ;
#6988 = ORIENTED_EDGE ( 'NONE', *, *, #889, .F. ) ;
#6989 = CARTESIAN_POINT ( 'NONE',  ( 9.048619709455110183, -15.70011763207404876, 16.29988236792595657 ) ) ;
#6990 = CARTESIAN_POINT ( 'NONE',  ( 0.000000000000000000, 0.000000000000000000, 21.00000000000000000 ) ) ;
#6991 = DIRECTION ( 'NONE',  ( -1.000000000000000000, 0.000000000000000000, -0.000000000000000000 ) ) ;
#6992 = CARTESIAN_POINT ( 'NONE',  ( 34.25000000000000000, 43.00000000000000000, 11.99999999999999645 ) ) ;
#6993 = AXIS2_PLACEMENT_3D ( 'NONE', #4511, #1484, #5340 ) ;
#6994 = PLANE ( 'NONE',  #5433 ) ;
#6995 = ORIENTED_EDGE ( 'NONE', *, *, #2186, .F. ) ;
#6996 = ORIENTED_EDGE ( 'NONE', *, *, #1190, .T. ) ;
#6997 = CARTESIAN_POINT ( 'NONE',  ( 4.000000000000000000, -18.47759065022712832, 7.653668647304757044 ) ) ;
#6998 = ORIENTED_EDGE ( 'NONE', *, *, #9221, .T. ) ;
#6999 = EDGE_CURVE ( 'NONE', #8041, #1701, #206, .T. ) ;
#7000 = LINE ( 'NONE', #7769, #5360 ) ;
#7001 = LINE ( 'NONE', #1765, #8866 ) ;
#7002 = EDGE_CURVE ( 'NONE', #7815, #8953, #8938, .T. ) ;
#7003 = ORIENTED_EDGE ( 'NONE', *, *, #6338, .F. ) ;
#7004 = CARTESIAN_POINT ( 'NONE',  ( 1.571166602479410136E-13, -22.50000000000000355, 5.000000000000000000 ) ) ;
#7005 = AXIS2_PLACEMENT_3D ( 'NONE', #7393, #1391, #2069 ) ;
#7006 = DIRECTION ( 'NONE',  ( 0.000000000000000000, 0.000000000000000000, -1.000000000000000000 ) ) ;
#7007 = CARTESIAN_POINT ( 'NONE',  ( 0.000000000000000000, -35.00000000000000000, 32.00000000000000000 ) ) ;
#7008 = FACE_OUTER_BOUND ( 'NONE', #7661, .T. ) ;
#7009 = CIRCLE ( 'NONE', #8994, 3.000000000000002665 ) ;
#7010 = ORIENTED_EDGE ( 'NONE', *, *, #9343, .T. ) ;
#7011 = VECTOR ( 'NONE', #8672, 1000.000000000000000 ) ;
#7012 = VERTEX_POINT ( 'NONE', #4194 ) ;
#7013 = CONICAL_SURFACE ( 'NONE', #9458, 18.50000000000001776, 0.7853981633974412846 ) ;
#7014 = ADVANCED_FACE ( 'NONE', ( #1941, #5554, #1894, #4962, #5743, #1990, #7121, #542, #1165, #2035, #5600, #4105, #4821, #494, #3468, #1305, #9232, #9379 ), #6413, .T. ) ;
#7015 = DIRECTION ( 'NONE',  ( -0.7071067811865460184, 0.000000000000000000, -0.7071067811865489050 ) ) ;
#7016 = AXIS2_PLACEMENT_3D ( 'NONE', #6174, #3138, #9041 ) ;
#7017 = CARTESIAN_POINT ( 'NONE',  ( -27.00000000000000000, 43.00000000000000000, 11.99999999999999645 ) ) ;
#7018 = DIRECTION ( 'NONE',  ( 0.7071067811865454633, -0.7071067811865494601, 0.000000000000000000 ) ) ;
#7019 = VECTOR ( 'NONE', #478, 1000.000000000000114 ) ;
#7020 = EDGE_CURVE ( 'NONE', #7294, #1809, #3423, .T. ) ;
#7021 = PLANE ( 'NONE',  #8183 ) ;
#7022 = AXIS2_PLACEMENT_3D ( 'NONE', #3805, #6749, #8943 ) ;
#7023 = EDGE_LOOP ( 'NONE', ( #6514, #4460, #3911, #5453 ) ) ;
#7024 = CIRCLE ( 'NONE', #1800, 5.000000000000000888 ) ;
#7025 = ORIENTED_EDGE ( 'NONE', *, *, #7654, .F. ) ;
#7026 = AXIS2_PLACEMENT_3D ( 'NONE', #8877, #6775, #1679 ) ;
#7027 = FACE_OUTER_BOUND ( 'NONE', #184, .T. ) ;
#7028 = DIRECTION ( 'NONE',  ( 1.000000000000000000, 0.000000000000000000, 0.000000000000000000 ) ) ;
#7029 = DIRECTION ( 'NONE',  ( -1.000000000000000000, -0.000000000000000000, -0.000000000000000000 ) ) ;
#7030 = LINE ( 'NONE', #6845, #6784 ) ;
#7031 = CARTESIAN_POINT ( 'NONE',  ( -40.00000000000000000, -30.00000000000000000, -13.00000000000000533 ) ) ;
#7032 = AXIS2_PLACEMENT_3D ( 'NONE', #6294, #9065, #3986 ) ;
#7033 = ORIENTED_EDGE ( 'NONE', *, *, #9339, .F. ) ;
#7034 = B_SPLINE_CURVE_WITH_KNOTS ( 'NONE', 3,
 ( #4845, #1274, #5670, #1189, #1967, #2643, #470, #1230, #4127, #4170, #513, #3441, #4211, #7140 ),
 .UNSPECIFIED., .F., .F.,
 ( 4, 2, 2, 2, 2, 2, 4 ),
 ( 0.000000000000000000, 0.002003588478668952722, 0.004007176957337905444, 0.005008971196672381589, 0.006010765436006858600, 0.007012559675341334745, 0.008014353914675810889 ),
 .UNSPECIFIED. ) ;
#7035 = EDGE_LOOP ( 'NONE', ( #6425, #8327 ) ) ;
#7036 = DIRECTION ( 'NONE',  ( 0.000000000000000000, -0.5469441386039887165, 0.8371691043312223801 ) ) ;
#7037 = ORIENTED_EDGE ( 'NONE', *, *, #2848, .F. ) ;
#7038 = DIRECTION ( 'NONE',  ( 0.7071067811865475727, -0.000000000000000000, 0.7071067811865475727 ) ) ;
#7039 = DIRECTION ( 'NONE',  ( -1.000000000000000000, 0.000000000000000000, 0.000000000000000000 ) ) ;
#7040 = ADVANCED_FACE ( 'NONE', ( #8480 ), #7756, .F. ) ;
#7041 = AXIS2_PLACEMENT_3D ( 'NONE', #5987, #3678, #6660 ) ;
#7042 = CARTESIAN_POINT ( 'NONE',  ( 2.265596578422601819E-15, -34.99999999999999289, 50.49999999999998579 ) ) ;
#7043 = DIRECTION ( 'NONE',  ( -1.000000000000000000, 0.000000000000000000, 0.000000000000000000 ) ) ;
#7044 = EDGE_CURVE ( 'NONE', #4833, #9400, #2189, .T. ) ;
#7045 = DIRECTION ( 'NONE',  ( 0.000000000000000000, 0.000000000000000000, -1.000000000000000000 ) ) ;
#7046 = ORIENTED_EDGE ( 'NONE', *, *, #8934, .F. ) ;
#7047 = ORIENTED_EDGE ( 'NONE', *, *, #3335, .F. ) ;
#7048 = DIRECTION ( 'NONE',  ( -0.000000000000000000, -1.000000000000000000, -0.000000000000000000 ) ) ;
#7049 = AXIS2_PLACEMENT_3D ( 'NONE', #5915, #5197, #1494 ) ;
#7050 = ORIENTED_EDGE ( 'NONE', *, *, #435, .F. ) ;
#7051 = DIRECTION ( 'NONE',  ( 0.000000000000000000, 1.000000000000000000, 0.000000000000000000 ) ) ;
#7052 = DIRECTION ( 'NONE',  ( -1.000000000000000000, -0.000000000000000000, -0.000000000000000000 ) ) ;
#7053 = ORIENTED_EDGE ( 'NONE', *, *, #9457, .F. ) ;
#7054 = PLANE ( 'NONE',  #705 ) ;
#7055 = CARTESIAN_POINT ( 'NONE',  ( 0.000000000000000000, -34.99999999999999289, 32.00000000000000000 ) ) ;
#7056 = LINE ( 'NONE', #7909, #6211 ) ;
#7057 = LINE ( 'NONE', #5524, #8095 ) ;
#7058 = ORIENTED_EDGE ( 'NONE', *, *, #3359, .F. ) ;
#7059 = ORIENTED_EDGE ( 'NONE', *, *, #4676, .T. ) ;
#7060 = EDGE_CURVE ( 'NONE', #8187, #8436, #8785, .T. ) ;
#7061 = ADVANCED_FACE ( 'NONE', ( #592 ), #4186, .F. ) ;
#7062 = DIRECTION ( 'NONE',  ( 0.000000000000000000, 0.000000000000000000, -1.000000000000000000 ) ) ;
#7063 = PLANE ( 'NONE',  #6807 ) ;
#7064 = FACE_OUTER_BOUND ( 'NONE', #6567, .T. ) ;
#7065 = ORIENTED_EDGE ( 'NONE', *, *, #5213, .F. ) ;
#7066 = ORIENTED_EDGE ( 'NONE', *, *, #9254, .T. ) ;
#7067 = ORIENTED_EDGE ( 'NONE', *, *, #6724, .T. ) ;
#7068 = AXIS2_PLACEMENT_3D ( 'NONE', #5032, #3537, #2912 ) ;
#7069 = ORIENTED_EDGE ( 'NONE', *, *, #7402, .T. ) ;
#7070 = CARTESIAN_POINT ( 'NONE',  ( -30.00000000000000000, 0.000000000000000000, 10.00000000000000000 ) ) ;
#7071 = DIRECTION ( 'NONE',  ( -1.000000000000000000, 0.000000000000000000, 0.000000000000000000 ) ) ;
#7072 = CYLINDRICAL_SURFACE ( 'NONE', #8892, 0.7500000000013684609 ) ;
#7073 = AXIS2_PLACEMENT_3D ( 'NONE', #2487, #7612, #4642 ) ;
#7074 =( LENGTH_UNIT ( ) NAMED_UNIT ( * ) SI_UNIT ( .MILLI., .METRE. ) );
#7075 = EDGE_LOOP ( 'NONE', ( #6757, #6472 ) ) ;
#7076 = ORIENTED_EDGE ( 'NONE', *, *, #7109, .F. ) ;
#7077 =( NAMED_UNIT ( * ) PLANE_ANGLE_UNIT ( ) SI_UNIT ( $, .RADIAN. ) );
#7078 = ORIENTED_EDGE ( 'NONE', *, *, #913, .F. ) ;
#7079 = CARTESIAN_POINT ( 'NONE',  ( 2.000000000000000000, 0.000000000000000000, 0.000000000000000000 ) ) ;
#7080 = CARTESIAN_POINT ( 'NONE',  ( 4.000000000000000000, 18.47759065022658120, 7.653668647302884764 ) ) ;
#7081 = CARTESIAN_POINT ( 'NONE',  ( 0.000000000000000000, 0.000000000000000000, 27.50000000000000355 ) ) ;
#7082 = CARTESIAN_POINT ( 'NONE',  ( 4.000000000000000000, 14.14213562373112154, -14.14213562373077870 ) ) ;
#7083 = VECTOR ( 'NONE', #6177, 999.9999999999998863 ) ;
#7084 = LINE ( 'NONE', #4743, #2822 ) ;
#7085 = ORIENTED_EDGE ( 'NONE', *, *, #3180, .F. ) ;
#7086 = VERTEX_POINT ( 'NONE', #7946 ) ;
#7087 = DIRECTION ( 'NONE',  ( 1.000000000000000000, 0.000000000000000000, -0.000000000000000000 ) ) ;
#7088 = ORIENTED_EDGE ( 'NONE', *, *, #6832, .T. ) ;
#7089 = DIRECTION ( 'NONE',  ( -0.000000000000000000, -0.000000000000000000, -1.000000000000000000 ) ) ;
#7090 = DIRECTION ( 'NONE',  ( -1.000000000000000000, 0.000000000000000000, 0.000000000000000000 ) ) ;
#7091 = LINE ( 'NONE', #654, #2405 ) ;
#7092 = CARTESIAN_POINT ( 'NONE',  ( 0.000000000000000000, 0.000000000000000000, 0.000000000000000000 ) ) ;
#7093 = CIRCLE ( 'NONE', #5266, 6.000000000000000000 ) ;
#7094 = CARTESIAN_POINT ( 'NONE',  ( -12.37436867076458036, -12.37436867076458036, 19.62563132923542142 ) ) ;
#7095 = CARTESIAN_POINT ( 'NONE',  ( 0.000000000000000000, -22.50000000000000355, 5.000000000000000000 ) ) ;
#7096 = ORIENTED_EDGE ( 'NONE', *, *, #8640, .F. ) ;
#7097 = ORIENTED_EDGE ( 'NONE', *, *, #2624, .F. ) ;
#7098 = AXIS2_PLACEMENT_3D ( 'NONE', #9189, #7849, #1214 ) ;
#7099 = DIRECTION ( 'NONE',  ( -1.000000000000000000, -0.000000000000000000, -0.000000000000000000 ) ) ;
#7100 = DIRECTION ( 'NONE',  ( 0.000000000000000000, 0.000000000000000000, -1.000000000000000000 ) ) ;
#7101 = CARTESIAN_POINT ( 'NONE',  ( -52.42476942962457542, 29.19763577280653877, -80.99738777760514097 ) ) ;
#7102 = ORIENTED_EDGE ( 'NONE', *, *, #137, .T. ) ;
#7103 = EDGE_LOOP ( 'NONE', ( #3282, #1999 ) ) ;
#7104 = ORIENTED_EDGE ( 'NONE', *, *, #2739, .F. ) ;
#7105 = ADVANCED_FACE ( 'NONE', ( #3378 ), #7717, .F. ) ;
#7106 = ORIENTED_EDGE ( 'NONE', *, *, #5881, .F. ) ;
#7107 = EDGE_CURVE ( 'NONE', #1500, #2573, #4800, .T. ) ;
#7108 = CARTESIAN_POINT ( 'NONE',  ( -26.99999999999998934, -29.99999999999999289, 64.00000000000000000 ) ) ;
#7109 = EDGE_CURVE ( 'NONE', #2056, #4903, #6035, .T. ) ;
#7110 = EDGE_CURVE ( 'NONE', #1940, #5539, #8780, .T. ) ;
#7111 = FACE_OUTER_BOUND ( 'NONE', #2774, .T. ) ;
#7112 = DIRECTION ( 'NONE',  ( 1.000000000000000000, -0.000000000000000000, -0.000000000000000000 ) ) ;
#7113 = CARTESIAN_POINT ( 'NONE',  ( -28.21791960234945051, -3.296518076058942093, 1.407948315796079486 ) ) ;
#7114 = VECTOR ( 'NONE', #4844, 1000.000000000000000 ) ;
#7115 = FACE_BOUND ( 'NONE', #6320, .T. ) ;
#7116 = ORIENTED_EDGE ( 'NONE', *, *, #9442, .T. ) ;
#7117 = LINE ( 'NONE', #538, #2416 ) ;
#7118 = AXIS2_PLACEMENT_3D ( 'NONE', #9143, #5461, #4020 ) ;
#7119 = DIRECTION ( 'NONE',  ( 1.000000000000000000, 0.000000000000000000, 0.000000000000000000 ) ) ;
#7120 = ORIENTED_EDGE ( 'NONE', *, *, #5553, .T. ) ;
#7121 = FACE_BOUND ( 'NONE', #1200, .T. ) ;
#7122 = PLANE ( 'NONE',  #2241 ) ;
#7123 = AXIS2_PLACEMENT_3D ( 'NONE', #7234, #2235, #9443 ) ;
#7124 = ADVANCED_FACE ( 'NONE', ( #4340, #67 ), #5254, .T. ) ;
#7125 = LINE ( 'NONE', #1943, #3387 ) ;
#7126 = AXIS2_PLACEMENT_3D ( 'NONE', #8360, #3894, #2412 ) ;
#7127 = LINE ( 'NONE', #9335, #2530 ) ;
#7128 = LINE ( 'NONE', #7761, #664 ) ;
#7129 = ORIENTED_EDGE ( 'NONE', *, *, #6688, .F. ) ;
#7130 = ADVANCED_FACE ( 'NONE', ( #3616 ), #6556, .T. ) ;
#7131 = ORIENTED_EDGE ( 'NONE', *, *, #1850, .F. ) ;
#7132 = FACE_OUTER_BOUND ( 'NONE', #6453, .T. ) ;
#7133 = ORIENTED_EDGE ( 'NONE', *, *, #9070, .F. ) ;
#7134 = CARTESIAN_POINT ( 'NONE',  ( 4.000000000000000000, -9.628187502531647418E-13, -19.99999999999950262 ) ) ;
#7135 = PLANE ( 'NONE',  #582 ) ;
#7136 = CARTESIAN_POINT ( 'NONE',  ( 19.00000000000000000, 0.000000000000000000, 0.000000000000000000 ) ) ;
#7137 = CARTESIAN_POINT ( 'NONE',  ( 16.00000000000000000, -43.00000000000000000, 11.99999999999999645 ) ) ;
#7138 = AXIS2_PLACEMENT_3D ( 'NONE', #5089, #5693, #3654 ) ;
#7139 = DIRECTION ( 'NONE',  ( 1.000000000000000000, 0.000000000000000000, 0.000000000000000000 ) ) ;
#7140 = CARTESIAN_POINT ( 'NONE',  ( 28.75000000000001776, 7.654042494438380704E-16, 1.750000000000019762 ) ) ;
#7141 = ORIENTED_EDGE ( 'NONE', *, *, #2262, .T. ) ;
#7142 = ORIENTED_EDGE ( 'NONE', *, *, #6366, .T. ) ;
#7143 = AXIS2_PLACEMENT_3D ( 'NONE', #8886, #5239, #5074 ) ;
#7144 = DIRECTION ( 'NONE',  ( -0.000000000000000000, -0.000000000000000000, 1.000000000000000000 ) ) ;
#7145 = PRODUCT_DEFINITION_SHAPE ( 'NONE', 'NONE',  #9501 ) ;
#7146 = DIRECTION ( 'NONE',  ( 1.000000000000000000, 0.000000000000000000, 0.000000000000000000 ) ) ;
#7147 = EDGE_CURVE ( 'NONE', #6634, #3040, #8895, .T. ) ;
#7148 = FACE_OUTER_BOUND ( 'NONE', #8856, .T. ) ;
#7149 = VECTOR ( 'NONE', #9292, 1000.000000000000114 ) ;
#7150 = CARTESIAN_POINT ( 'NONE',  ( -0.7500000000000000000, 0.7500000000000000000, 1.500000000000000000 ) ) ;
#7151 = CARTESIAN_POINT ( 'NONE',  ( 3.499999999999999556, 2.755455298081544778E-15, -22.50000000000000000 ) ) ;
#7152 = ORIENTED_EDGE ( 'NONE', *, *, #3309, .T. ) ;
#7153 = EDGE_CURVE ( 'NONE', #2851, #4799, #7093, .T. ) ;
#7154 = ORIENTED_EDGE ( 'NONE', *, *, #4051, .T. ) ;
#7155 = ORIENTED_EDGE ( 'NONE', *, *, #8116, .F. ) ;
#7156 = ORIENTED_EDGE ( 'NONE', *, *, #3828, .F. ) ;
#7157 = AXIS2_PLACEMENT_3D ( 'NONE', #7757, #7039, #779 ) ;
#7158 = CARTESIAN_POINT ( 'NONE',  ( -31.99999999999999289, -29.99999999999996447, 5.000000000000004441 ) ) ;
#7159 = CARTESIAN_POINT ( 'NONE',  ( -3.500000000000000000, 4.119968255444916849E-15, 1.500000000000000000 ) ) ;
#7160 = DIRECTION ( 'NONE',  ( 1.000000000000000000, 0.000000000000000000, 0.000000000000000000 ) ) ;
#7161 = CIRCLE ( 'NONE', #3331, 1.560000000001265263 ) ;
#7162 = CARTESIAN_POINT ( 'NONE',  ( -26.79453276911117854, -6.186305604711966666, 0.4929139230000563754 ) ) ;
#7163 = COLOUR_RGB ( '',0.7921568627450980005, 0.8196078431372548767, 0.9333333333333333481 ) ;
#7164 = VECTOR ( 'NONE', #6923, 999.9999999999998863 ) ;
#7165 = LINE ( 'NONE', #7259, #7930 ) ;
#7166 = AXIS2_PLACEMENT_3D ( 'NONE', #4986, #7336, #4218 ) ;
#7167 = ORIENTED_EDGE ( 'NONE', *, *, #8816, .F. ) ;
#7168 = CARTESIAN_POINT ( 'NONE',  ( -31.99999999999999289, 29.99999999999997868, 64.00000000000000000 ) ) ;
#7169 = EDGE_LOOP ( 'NONE', ( #1559, #8742, #363, #6059 ) ) ;
#7170 = DIRECTION ( 'NONE',  ( -1.000000000000000000, 0.000000000000000000, 0.000000000000000000 ) ) ;
#7171 = CARTESIAN_POINT ( 'NONE',  ( 17.50000000000000355, 0.000000000000000000, 63.00000000000002842 ) ) ;
#7172 = VECTOR ( 'NONE', #430, 1000.000000000000000 ) ;
#7174 = EDGE_CURVE ( 'NONE', #5769, #6494, #8628, .T. ) ;
#7173 = CARTESIAN_POINT ( 'NONE',  ( -26.99999999999998934, 35.00000000000000000, 59.00000000000000000 ) ) ;
#7175 = VECTOR ( 'NONE', #5029, 1000.000000000000000 ) ;
#7176 = DIRECTION ( 'NONE',  ( 1.000000000000000000, 0.000000000000000000, 0.000000000000000000 ) ) ;
#7177 = DIRECTION ( 'NONE',  ( -1.000000000000000000, 0.000000000000000000, 0.000000000000000000 ) ) ;
#7178 = ORIENTED_EDGE ( 'NONE', *, *, #4842, .F. ) ;
#7179 = VERTEX_POINT ( 'NONE', #3760 ) ;
#7180 = CARTESIAN_POINT ( 'NONE',  ( 4.000000000000000000, 14.14213562373112154, -12.58213562373077821 ) ) ;
#7181 = ORIENTED_EDGE ( 'NONE', *, *, #6534, .F. ) ;
#7182 = CARTESIAN_POINT ( 'NONE',  ( 27.00000000000000355, 29.99999999999997158, -3.066586833366757151E-16 ) ) ;
#7183 = DIRECTION ( 'NONE',  ( 0.000000000000000000, 0.000000000000000000, -1.000000000000000000 ) ) ;
#7184 = AXIS2_PLACEMENT_3D ( 'NONE', #2485, #6228, #2576 ) ;
#7185 = AXIS2_PLACEMENT_3D ( 'NONE', #8381, #1704, #6852 ) ;
#7186 = LINE ( 'NONE', #4353, #3166 ) ;
#7187 = FACE_OUTER_BOUND ( 'NONE', #1814, .T. ) ;
#7188 = DIRECTION ( 'NONE',  ( 0.000000000000000000, 0.000000000000000000, 1.000000000000000000 ) ) ;
#7189 = CONICAL_SURFACE ( 'NONE', #3057, 18.50000000000001776, 0.7853981633974412846 ) ;
#7190 = DIRECTION ( 'NONE',  ( -1.000000000000000000, -0.000000000000000000, -0.000000000000000000 ) ) ;
#7191 = ORIENTED_EDGE ( 'NONE', *, *, #3833, .T. ) ;
#7192 = AXIS2_PLACEMENT_3D ( 'NONE', #260, #8280, #3187 ) ;
#7193 = ORIENTED_EDGE ( 'NONE', *, *, #805, .F. ) ;
#7194 = CARTESIAN_POINT ( 'NONE',  ( 5.000000000000000000, 14.14213562373247868, 14.14213562373282329 ) ) ;
#7195 = ITEM_DEFINED_TRANSFORMATION ( 'NONE', 'NONE', #1772,  #1614 ) ;
#7196 = B_SPLINE_CURVE_WITH_KNOTS ( 'NONE', 3,
 ( #1991, #7947, #2713, #2080, #8613, #1259, #6508, #5696, #7804, #9234, #7850, #1306 ),
 .UNSPECIFIED., .F., .F.,
 ( 4, 2, 2, 2, 2, 4 ),
 ( 0.005117570262457497680, 0.006390849577664777653, 0.007027489235268418941, 0.007664128892872060228, 0.008937408208079342803, 0.01021068752328662538 ),
 .UNSPECIFIED. ) ;
#7197 = LINE ( 'NONE', #3644, #8093 ) ;
#7198 = DIRECTION ( 'NONE',  ( 1.000000000000000000, 0.000000000000000000, 0.000000000000000000 ) ) ;
#7199 = CARTESIAN_POINT ( 'NONE',  ( 53.29490495164537833, -15.90990257669733943, -54.09009742330271564 ) ) ;
#7200 = ORIENTED_EDGE ( 'NONE', *, *, #8251, .T. ) ;
#7201 = ORIENTED_EDGE ( 'NONE', *, *, #5424, .T. ) ;
#7202 = ORIENTED_EDGE ( 'NONE', *, *, #7706, .T. ) ;
#7203 = CIRCLE ( 'NONE', #9350, 18.49999999999997513 ) ;
#7204 =( BOUNDED_CURVE ( )  B_SPLINE_CURVE ( 3, ( #2633, #4160, #3432, #603 ),
 .UNSPECIFIED., .F., .F. ) 
 B_SPLINE_CURVE_WITH_KNOTS ( ( 4, 4 ),
 ( 4.712388980384689674, 7.853981633974482790 ),
 .UNSPECIFIED. ) 
 CURVE ( )  GEOMETRIC_REPRESENTATION_ITEM ( )  RATIONAL_B_SPLINE_CURVE ( ( 1.000000000000000000, 0.3333333333333333703, 0.3333333333333333703, 1.000000000000000000 ) ) 
 REPRESENTATION_ITEM ( '' )  );
#7205 = ORIENTED_EDGE ( 'NONE', *, *, #7365, .F. ) ;
#7206 = DIRECTION ( 'NONE',  ( -0.000000000000000000, -0.000000000000000000, -1.000000000000000000 ) ) ;
#7207 = CARTESIAN_POINT ( 'NONE',  ( -15.99999999999999822, -20.99999999999999289, -16.89999999999999858 ) ) ;
#7208 = ADVANCED_FACE ( 'NONE', ( #2899 ), #4180, .T. ) ;
#7209 = DIRECTION ( 'NONE',  ( -1.000000000000000000, -0.000000000000000000, -0.000000000000000000 ) ) ;
#7210 = CARTESIAN_POINT ( 'NONE',  ( -27.45147183906051680, -5.102343880922198593, 0.9152318965389161232 ) ) ;
#7211 = CARTESIAN_POINT ( 'NONE',  ( 0.000000000000000000, 0.000000000000000000, 0.000000000000000000 ) ) ;
#7212 = ORIENTED_EDGE ( 'NONE', *, *, #6754, .T. ) ;
#7213 = CARTESIAN_POINT ( 'NONE',  ( 27.00000000000000000, 43.00000000000000000, 11.99999999999999645 ) ) ;
#7214 = ORIENTED_EDGE ( 'NONE', *, *, #1713, .T. ) ;
#7215 = DIRECTION ( 'NONE',  ( 0.000000000000000000, 0.000000000000000000, 1.000000000000000000 ) ) ;
#7216 = EDGE_CURVE ( 'NONE', #8325, #7845, #3028, .T. ) ;
#7217 = DIRECTION ( 'NONE',  ( -0.000000000000000000, -0.000000000000000000, -1.000000000000000000 ) ) ;
#7218 = VECTOR ( 'NONE', #1754, 1000.000000000000000 ) ;
#7219 = LINE ( 'NONE', #9429, #8432 ) ;
#7220 = CARTESIAN_POINT ( 'NONE',  ( 37.00000000000000000, 13.96446609406729777, -95.00000000000000000 ) ) ;
#7221 = LINE ( 'NONE', #8668, #4347 ) ;
#7222 = EDGE_LOOP ( 'NONE', ( #45, #8434 ) ) ;
#7223 = EDGE_LOOP ( 'NONE', ( #5901, #2771, #8022, #577 ) ) ;
#7224 = CARTESIAN_POINT ( 'NONE',  ( -38.00000000000000711, 43.00000000000000000, 11.99999999999999645 ) ) ;
#7225 = ORIENTED_EDGE ( 'NONE', *, *, #7768, .T. ) ;
#7226 = DIRECTION ( 'NONE',  ( 0.000000000000000000, 0.000000000000000000, 1.000000000000000000 ) ) ;
#7227 = ADVANCED_FACE ( 'NONE', ( #5061, #2988 ), #5832, .T. ) ;
#7228 = CARTESIAN_POINT ( 'NONE',  ( -2.499999999999998668, 0.000000000000000000, 21.00000000000000000 ) ) ;
#7229 = CARTESIAN_POINT ( 'NONE',  ( -12.55753963192698741, 30.00000000000000000, -8.879521428754452828 ) ) ;
#7230 = EDGE_CURVE ( 'NONE', #4290, #2562, #1371, .T. ) ;
#7231 = EDGE_CURVE ( 'NONE', #8166, #6868, #5618, .T. ) ;
#7232 = EDGE_CURVE ( 'NONE', #7477, #1471, #5727, .T. ) ;
#7233 = FACE_BOUND ( 'NONE', #1607, .T. ) ;
#7234 = CARTESIAN_POINT ( 'NONE',  ( 0.000000000000000000, 0.000000000000000000, 25.00000000000000000 ) ) ;
#7235 = DIRECTION ( 'NONE',  ( 0.000000000000000000, 0.000000000000000000, 1.000000000000000000 ) ) ;
#7236 = ORIENTED_EDGE ( 'NONE', *, *, #1912, .F. ) ;
#7237 = ORIENTED_EDGE ( 'NONE', *, *, #1218, .T. ) ;
#7238 = VECTOR ( 'NONE', #8172, 1000.000000000000000 ) ;
#7239 = DIRECTION ( 'NONE',  ( -1.000000000000000000, -0.000000000000000000, -0.000000000000000000 ) ) ;
#7240 = CONTEXT_DEPENDENT_SHAPE_REPRESENTATION ( #6712, #7145 ) ;
#7241 = ADVANCED_FACE ( 'NONE', ( #4384 ), #736, .T. ) ;
#7242 = VECTOR ( 'NONE', #2612, 1000.000000000000000 ) ;
#7243 = ADVANCED_FACE ( 'NONE', ( #3669 ), #5204, .F. ) ;
#7244 = CARTESIAN_POINT ( 'NONE',  ( 0.000000000000000000, 0.000000000000000000, 28.50000000000000355 ) ) ;
#7245 = ADVANCED_FACE ( 'NONE', ( #8138, #4480 ), #639, .F. ) ;
#7246 = LINE ( 'NONE', #1626, #7568 ) ;
#7247 = CARTESIAN_POINT ( 'NONE',  ( 0.000000000000000000, 0.000000000000000000, 11.00000000000000000 ) ) ;
#7248 = ORIENTED_EDGE ( 'NONE', *, *, #4232, .T. ) ;
#7249 = EDGE_LOOP ( 'NONE', ( #2951, #699 ) ) ;
#7250 = AXIS2_PLACEMENT_3D ( 'NONE', #936, #356, #3240 ) ;
#7251 = VERTEX_POINT ( 'NONE', #6125 ) ;
#7252 = ORIENTED_EDGE ( 'NONE', *, *, #4238, .T. ) ;
#7253 = DIRECTION ( 'NONE',  ( -1.000000000000000000, 0.000000000000000000, 0.000000000000000000 ) ) ;
#7254 = LINE ( 'NONE', #8836, #8100 ) ;
#7255 = DIRECTION ( 'NONE',  ( -0.000000000000000000, -0.000000000000000000, -1.000000000000000000 ) ) ;
#7256 = AXIS2_PLACEMENT_3D ( 'NONE', #1591, #1312, #5836 ) ;
#7257 = CARTESIAN_POINT ( 'NONE',  ( 19.00000000000000000, 0.000000000000000000, 13.66147716702868031 ) ) ;
#7258 = CARTESIAN_POINT ( 'NONE',  ( -31.99999999999999289, 29.99999999999997868, 58.99999999999997158 ) ) ;
#7259 = CARTESIAN_POINT ( 'NONE',  ( 29.50000000000000711, 32.49999999999999289, 5.000000000000018652 ) ) ;
#7260 = ORIENTED_EDGE ( 'NONE', *, *, #5540, .F. ) ;
#7261 = CARTESIAN_POINT ( 'NONE',  ( 60.00000000000000000, -15.90990257669733943, -57.09009742330271564 ) ) ;
#7262 = ORIENTED_EDGE ( 'NONE', *, *, #2823, .T. ) ;
#7263 = DIRECTION ( 'NONE',  ( 1.000000000000000000, 0.000000000000000000, 0.000000000000000000 ) ) ;
#7264 = DIRECTION ( 'NONE',  ( 0.7071067811865444641, -0.7071067811865505703, -0.000000000000000000 ) ) ;
#7265 = DIRECTION ( 'NONE',  ( -0.000000000000000000, -0.000000000000000000, -1.000000000000000000 ) ) ;
#7266 = AXIS2_PLACEMENT_3D ( 'NONE', #3885, #6106, #7682 ) ;
#7267 = CARTESIAN_POINT ( 'NONE',  ( -0.7500000000000000000, 0.7500000000000000000, 1.500000000000000000 ) ) ;
#7268 = DIRECTION ( 'NONE',  ( -0.000000000000000000, -0.000000000000000000, -1.000000000000000000 ) ) ;
#7269 = ORIENTED_EDGE ( 'NONE', *, *, #847, .T. ) ;
#7270 = ORIENTED_EDGE ( 'NONE', *, *, #2413, .F. ) ;
#7271 = CARTESIAN_POINT ( 'NONE',  ( 2.254970896015934478, 28.06387613437634343, 1.153664892585073654 ) ) ;
#7272 = ORIENTED_EDGE ( 'NONE', *, *, #2836, .T. ) ;
#7273 = CARTESIAN_POINT ( 'NONE',  ( -53.29490495164537833, 27.56180520566615044, -41.61356529332876875 ) ) ;
#7274 = CIRCLE ( 'NONE', #4681, 17.50000000000000000 ) ;
#7275 = CARTESIAN_POINT ( 'NONE',  ( -31.99999999999999289, -34.99999999999999289, 64.00000000000000000 ) ) ;
#7276 = CARTESIAN_POINT ( 'NONE',  ( 32.83333333333333570, -21.66666666666668206, -90.83333333333332860 ) ) ;
#7277 = AXIS2_PLACEMENT_3D ( 'NONE', #7567, #1709, #7471 ) ;
#7278 = LINE ( 'NONE', #6521, #6467 ) ;
#7279 = CARTESIAN_POINT ( 'NONE',  ( -19.62310601229373930, -19.62310601229373930, 37.12563132923541076 ) ) ;
#7280 = CARTESIAN_POINT ( 'NONE',  ( -53.29490495164537833, -1.836970198721028011E-15, -85.00000000000000000 ) ) ;
#7281 = EDGE_CURVE ( 'NONE', #2677, #1076, #6933, .T. ) ;
#7282 = ORIENTED_EDGE ( 'NONE', *, *, #8299, .F. ) ;
#7283 = ORIENTED_EDGE ( 'NONE', *, *, #5299, .T. ) ;
#7284 = ADVANCED_FACE ( 'NONE', ( #4582 ), #7452, .T. ) ;
#7285 = DIRECTION ( 'NONE',  ( 0.7071067811865486830, 8.659560562354948882E-17, -0.7071067811865464625 ) ) ;
#7286 = DIRECTION ( 'NONE',  ( -0.000000000000000000, 1.000000000000000000, -0.000000000000000000 ) ) ;
#7287 =( GEOMETRIC_REPRESENTATION_CONTEXT ( 3 ) GLOBAL_UNCERTAINTY_ASSIGNED_CONTEXT ( ( #92 ) ) GLOBAL_UNIT_ASSIGNED_CONTEXT ( ( #7663, #8379, #3096 ) ) REPRESENTATION_CONTEXT ( 'NONE', 'WORKASPACE' ) );
#7288 = DIRECTION ( 'NONE',  ( -0.7071067811865525687, 8.659560562354873694E-17, -0.7071067811865425767 ) ) ;
#7289 = ADVANCED_FACE ( 'NONE', ( #2565 ), #7553, .F. ) ;
#7290 = CARTESIAN_POINT ( 'NONE',  ( 27.00000000000000355, -29.99999999999996447, 0.000000000000000000 ) ) ;
#7291 = FACE_OUTER_BOUND ( 'NONE', #7529, .T. ) ;
#7292 = ORIENTED_EDGE ( 'NONE', *, *, #7545, .T. ) ;
#7293 = ORIENTED_EDGE ( 'NONE', *, *, #4461, .F. ) ;
#7294 = VERTEX_POINT ( 'NONE', #5446 ) ;
#7295 = DIRECTION ( 'NONE',  ( 0.000000000000000000, -0.7071067811865807684, 0.7071067811865143771 ) ) ;
#7296 = EDGE_CURVE ( 'NONE', #5309, #6840, #6751, .T. ) ;
#7297 = ORIENTED_EDGE ( 'NONE', *, *, #21, .F. ) ;
#7298 = CARTESIAN_POINT ( 'NONE',  ( -37.00000000000000711, -15.90990257669733943, -85.90990257669729147 ) ) ;
#7299 = DIRECTION ( 'NONE',  ( 0.000000000000000000, 0.000000000000000000, 1.000000000000000000 ) ) ;
#7300 = VECTOR ( 'NONE', #3483, 1000.000000000000114 ) ;
#7301 = DIRECTION ( 'NONE',  ( 0.000000000000000000, 0.000000000000000000, -1.000000000000000000 ) ) ;
#7302 = PRODUCT_DEFINITION_SHAPE ( 'NONE', 'NONE',  #2939 ) ;
#7303 = CARTESIAN_POINT ( 'NONE',  ( -31.99999999999999289, -34.99999999999999289, 64.00000000000000000 ) ) ;
#7304 = DIRECTION ( 'NONE',  ( 0.000000000000000000, 0.000000000000000000, -1.000000000000000000 ) ) ;
#7305 = FACE_BOUND ( 'NONE', #2972, .T. ) ;
#7306 = EDGE_LOOP ( 'NONE', ( #6031, #2021, #5716, #8167, #7511 ) ) ;
#7307 = AXIS2_PLACEMENT_3D ( 'NONE', #6990, #3198, #9003 ) ;
#7308 = AXIS2_PLACEMENT_3D ( 'NONE', #1903, #2678, #9242 ) ;
#7309 = CARTESIAN_POINT ( 'NONE',  ( 26.21170834203230982, 53.97171801779368394, -2.612255525622733554 ) ) ;
#7310 = ORIENTED_EDGE ( 'NONE', *, *, #6651, .F. ) ;
#7311 = DIRECTION ( 'NONE',  ( 0.000000000000000000, 0.000000000000000000, -1.000000000000000000 ) ) ;
#7312 = DIRECTION ( 'NONE',  ( -1.000000000000000000, 0.000000000000000000, 0.000000000000000000 ) ) ;
#7313 = CARTESIAN_POINT ( 'NONE',  ( -31.99999999999999289, -34.99999999999999289, 58.99999999999997158 ) ) ;
#7314 = AXIS2_PLACEMENT_3D ( 'NONE', #686, #6536, #25 ) ;
#7315 = CARTESIAN_POINT ( 'NONE',  ( 31.00000000000002132, 0.000000000000000000, 32.00000000000000000 ) ) ;
#7316 = AXIS2_PLACEMENT_3D ( 'NONE', #6019, #8940, #2744 ) ;
#7317 = ORIENTED_EDGE ( 'NONE', *, *, #5368, .F. ) ;
#7318 = AXIS2_PLACEMENT_3D ( 'NONE', #1690, #2556, #6121 ) ;
#7319 = ORIENTED_EDGE ( 'NONE', *, *, #6266, .T. ) ;
#7320 = CARTESIAN_POINT ( 'NONE',  ( 0.000000000000000000, 0.000000000000000000, 50.00000000000000000 ) ) ;
#7321 = AXIS2_PLACEMENT_3D ( 'NONE', #8223, #8985, #1646 ) ;
#7322 = VERTEX_POINT ( 'NONE', #8945 ) ;
#7323 = EDGE_CURVE ( 'NONE', #991, #8987, #970, .T. ) ;
#7324 = AXIS2_PLACEMENT_3D ( 'NONE', #4428, #7299, #8887 ) ;
#7325 = CARTESIAN_POINT ( 'NONE',  ( 26.02777777777776791, 7.180166011355005651, 0.000000000000000000 ) ) ;
#7326 = DIRECTION ( 'NONE',  ( -1.000000000000000000, 0.000000000000000000, 0.000000000000000000 ) ) ;
#7327 = DIRECTION ( 'NONE',  ( 0.000000000000000000, 0.000000000000000000, 1.000000000000000000 ) ) ;
#7328 = ADVANCED_FACE ( 'NONE', ( #2375 ), #1018, .F. ) ;
#7329 = DIRECTION ( 'NONE',  ( 0.000000000000000000, 0.000000000000000000, 1.000000000000000000 ) ) ;
#7330 = LINE ( 'NONE', #4311, #8810 ) ;
#7331 = PLANE ( 'NONE',  #5589 ) ;
#7332 = ORIENTED_EDGE ( 'NONE', *, *, #4128, .T. ) ;
#7333 = ORIENTED_EDGE ( 'NONE', *, *, #2959, .T. ) ;
#7334 = DIRECTION ( 'NONE',  ( 0.000000000000000000, 0.000000000000000000, -1.000000000000000000 ) ) ;
#7335 = FACE_OUTER_BOUND ( 'NONE', #7401, .T. ) ;
#7336 = DIRECTION ( 'NONE',  ( 0.000000000000000000, 0.000000000000000000, -1.000000000000000000 ) ) ;
#7337 = AXIS2_PLACEMENT_3D ( 'NONE', #7623, #1044, #3984 ) ;
#7338 = FACE_BOUND ( 'NONE', #4661, .T. ) ;
#7339 = CARTESIAN_POINT ( 'NONE',  ( -31.99999999999999289, 0.000000000000000000, 32.00000000000000000 ) ) ;
#7340 = ORIENTED_EDGE ( 'NONE', *, *, #1218, .F. ) ;
#7341 = ORIENTED_EDGE ( 'NONE', *, *, #3471, .T. ) ;
#7342 = PRODUCT_RELATED_PRODUCT_CATEGORY ( 'part', '', ( #6699 ) ) ;
#7343 = VERTEX_POINT ( 'NONE', #4003 ) ;
#7344 = EDGE_CURVE ( 'NONE', #4223, #2372, #8226, .T. ) ;
#7345 = CARTESIAN_POINT ( 'NONE',  ( -8.230900400053725363, 17.56495618815237947, 61.81275442470098369 ) ) ;
#7346 = ORIENTED_EDGE ( 'NONE', *, *, #5814, .F. ) ;
#7347 = EDGE_CURVE ( 'NONE', #7012, #1699, #9040, .T. ) ;
#7348 = ADVANCED_FACE ( 'NONE', ( #1739 ), #3857, .T. ) ;
#7349 = CARTESIAN_POINT ( 'NONE',  ( -0.7500000000000000000, 0.7500000000000000000, 1.500000000000000000 ) ) ;
#7350 = DIRECTION ( 'NONE',  ( -1.000000000000000000, -0.000000000000000000, -0.000000000000000000 ) ) ;
#7351 = EDGE_CURVE ( 'NONE', #7415, #4522, #6189, .T. ) ;
#7352 = DIRECTION ( 'NONE',  ( -1.000000000000000000, 0.000000000000000000, 0.000000000000000000 ) ) ;
#7353 = DIRECTION ( 'NONE',  ( 1.000000000000000000, 0.000000000000000000, 0.000000000000000000 ) ) ;
#7354 = CARTESIAN_POINT ( 'NONE',  ( 0.000000000000000000, 22.50000000000000355, 5.000000000000000000 ) ) ;
#7355 = DIRECTION ( 'NONE',  ( -1.000000000000000000, 0.000000000000000000, 0.000000000000000000 ) ) ;
#7356 = ORIENTED_EDGE ( 'NONE', *, *, #9403, .T. ) ;
#7357 = CARTESIAN_POINT ( 'NONE',  ( 0.000000000000000000, 22.50000000000000355, 0.000000000000000000 ) ) ;
#7358 = EDGE_CURVE ( 'NONE', #4158, #7976, #4677, .T. ) ;
#7359 = ORIENTED_EDGE ( 'NONE', *, *, #6709, .F. ) ;
#7360 = CARTESIAN_POINT ( 'NONE',  ( 12.37436867076458036, -12.37436867076458036, 44.37436867076458213 ) ) ;
#7361 = DIRECTION ( 'NONE',  ( 1.000000000000000000, 0.000000000000000000, 0.000000000000000000 ) ) ;
#7362 = EDGE_CURVE ( 'NONE', #4533, #6722, #6641, .T. ) ;
#7363 = PLANE ( 'NONE',  #748 ) ;
#7364 = DIRECTION ( 'NONE',  ( -0.000000000000000000, -0.000000000000000000, 1.000000000000000000 ) ) ;
#7365 = EDGE_CURVE ( 'NONE', #763, #7578, #6172, .T. ) ;
#7366 = VERTEX_POINT ( 'NONE', #2514 ) ;
#7367 = VERTEX_POINT ( 'NONE', #3903 ) ;
#7368 = DIRECTION ( 'NONE',  ( -0.000000000000000000, -0.000000000000000000, -1.000000000000000000 ) ) ;
#7369 = ORIENTED_EDGE ( 'NONE', *, *, #5924, .T. ) ;
#7370 = CARTESIAN_POINT ( 'NONE',  ( -60.00000000000000000, 0.000000000000000000, -30.00000000000000000 ) ) ;
#7371 = DIRECTION ( 'NONE',  ( 0.7071067811865505703, 0.7071067811865444641, -0.000000000000000000 ) ) ;
#7372 = AXIS2_PLACEMENT_3D ( 'NONE', #9236, #1167, #4019 ) ;
#7373 = CARTESIAN_POINT ( 'NONE',  ( 60.00000000000000000, 15.90990257669733943, -57.09009742330271564 ) ) ;
#7374 = LINE ( 'NONE', #4493, #3690 ) ;
#7375 = DIRECTION ( 'NONE',  ( -1.000000000000000000, -0.000000000000000000, -0.000000000000000000 ) ) ;
#7376 = CARTESIAN_POINT ( 'NONE',  ( -47.45689247961085044, -13.88265003728722924, -103.3380124720345350 ) ) ;
#7377 = CARTESIAN_POINT ( 'NONE',  ( 28.50000000000000355, 2.364097784513999692E-13, 5.000000000000000000 ) ) ;
#7378 = ORIENTED_EDGE ( 'NONE', *, *, #5666, .T. ) ;
#7379 = ORIENTED_EDGE ( 'NONE', *, *, #488, .T. ) ;
#7380 = DIRECTION ( 'NONE',  ( 0.000000000000000000, 0.000000000000000000, 1.000000000000000000 ) ) ;
#7381 = CYLINDRICAL_SURFACE ( 'NONE', #7950, 17.50000000000000355 ) ;
#7382 = VERTEX_POINT ( 'NONE', #8370 ) ;
#7383 = CIRCLE ( 'NONE', #8920, 30.00000000000000000 ) ;
#7384 = PRODUCT ( '6-M6-16', '6-M6-16', '', ( #244 ) ) ;
#7385 = CARTESIAN_POINT ( 'NONE',  ( 29.50000000000000711, 29.99999999999997513, 61.49999999999998579 ) ) ;
#7386 = EDGE_CURVE ( 'NONE', #6538, #7697, #6489, .T. ) ;
#7387 = FACE_BOUND ( 'NONE', #9072, .T. ) ;
#7388 = UNCERTAINTY_MEASURE_WITH_UNIT (LENGTH_MEASURE( 1.000000000000000082E-05 ), #7074, 'distance_accuracy_value', 'NONE');
#7389 = CARTESIAN_POINT ( 'NONE',  ( -9.364477336218591574, 62.15368297487812299, 0.9332626224471912701 ) ) ;
#7390 = VECTOR ( 'NONE', #2932, 1000.000000000000000 ) ;
#7391 = ORIENTED_EDGE ( 'NONE', *, *, #3530, .F. ) ;
#7392 = EDGE_LOOP ( 'NONE', ( #6484, #335, #5298, #5425, #766, #4000, #7889, #7033, #5355, #8620, #5455, #6197 ) ) ;
#7393 = CARTESIAN_POINT ( 'NONE',  ( -53.29490495164537833, -15.90990257669733943, -54.09009742330271564 ) ) ;
#7394 = CARTESIAN_POINT ( 'NONE',  ( 5.000000000000000000, 18.47759065022658120, 8.403668647301545391 ) ) ;
#7395 = CARTESIAN_POINT ( 'NONE',  ( 0.000000000000000000, 22.50000000000000355, 2.000000000000013767 ) ) ;
#7396 = CYLINDRICAL_SURFACE ( 'NONE', #5719, 3.000000000000002665 ) ;
#7397 = CIRCLE ( 'NONE', #3406, 2.999999999999999112 ) ;
#7398 = FACE_OUTER_BOUND ( 'NONE', #7787, .T. ) ;
#7399 = EDGE_CURVE ( 'NONE', #1766, #450, #7397, .T. ) ;
#7400 = DIRECTION ( 'NONE',  ( 0.000000000000000000, 0.000000000000000000, -1.000000000000000000 ) ) ;
#7401 = EDGE_LOOP ( 'NONE', ( #7955, #1411, #3577, #46 ) ) ;
#7402 = EDGE_CURVE ( 'NONE', #8405, #2113, #3722, .T. ) ;
#7403 = EDGE_CURVE ( 'NONE', #602, #3367, #8467, .T. ) ;
#7404 = EDGE_CURVE ( 'NONE', #2905, #975, #2655, .T. ) ;
#7405 = VERTEX_POINT ( 'NONE', #5635 ) ;
#7406 = CARTESIAN_POINT ( 'NONE',  ( 38.00000000000000000, -21.00000000000000000, -16.89999999999999858 ) ) ;
#7407 = DIRECTION ( 'NONE',  ( 0.000000000000000000, 0.000000000000000000, -1.000000000000000000 ) ) ;
#7408 = AXIS2_PLACEMENT_3D ( 'NONE', #501, #7501, #9431 ) ;
#7409 = FACE_OUTER_BOUND ( 'NONE', #9104, .T. ) ;
#7410 = VECTOR ( 'NONE', #7531, 1000.000000000000000 ) ;
#7411 = LINE ( 'NONE', #71, #2018 ) ;
#7412 = EDGE_LOOP ( 'NONE', ( #904, #66, #5837, #1858 ) ) ;
#7413 = ORIENTED_EDGE ( 'NONE', *, *, #6999, .T. ) ;
#7414 = CIRCLE ( 'NONE', #4963, 3.000000000000002665 ) ;
#7415 = VERTEX_POINT ( 'NONE', #4905 ) ;
#7416 = ORIENTED_EDGE ( 'NONE', *, *, #2533, .T. ) ;
#7417 = DIRECTION ( 'NONE',  ( -1.000000000000000000, 0.000000000000000000, 0.000000000000000000 ) ) ;
#7418 = ADVANCED_FACE ( 'NONE', ( #3456, #7027 ), #4184, .F. ) ;
#7419 = CARTESIAN_POINT ( 'NONE',  ( 27.00000000000000000, -43.00000000000000000, 11.99999999999999645 ) ) ;
#7420 = DIRECTION ( 'NONE',  ( 1.000000000000000000, 0.000000000000000000, 0.000000000000000000 ) ) ;
#7421 = CARTESIAN_POINT ( 'NONE',  ( 16.00000000000000000, -43.00000000000000000, 11.99999999999999645 ) ) ;
#7422 = EDGE_CURVE ( 'NONE', #6094, #2294, #4950, .T. ) ;
#7423 = DIRECTION ( 'NONE',  ( 0.000000000000000000, 1.000000000000000000, 0.000000000000000000 ) ) ;
#7424 = CYLINDRICAL_SURFACE ( 'NONE', #9098, 2.999999999999999112 ) ;
#7425 = ORIENTED_EDGE ( 'NONE', *, *, #3218, .F. ) ;
#7426 = CIRCLE ( 'NONE', #5282, 26.99999999999999645 ) ;
#7427 = ORIENTED_EDGE ( 'NONE', *, *, #5463, .F. ) ;
#7428 = DIRECTION ( 'NONE',  ( 1.000000000000000000, 0.000000000000000000, 0.000000000000000000 ) ) ;
#7429 = CIRCLE ( 'NONE', #6064, 6.000000000000000888 ) ;
#7430 = ORIENTED_EDGE ( 'NONE', *, *, #3258, .T. ) ;
#7431 = B_SPLINE_CURVE_WITH_KNOTS ( 'NONE', 3,
 ( #2758, #2029, #7162, #7210, #1395, #9373, #7113, #9322, #2706, #4333, #6502, #2799, #9420, #7932 ),
 .UNSPECIFIED., .F., .F.,
 ( 4, 2, 2, 2, 2, 2, 4 ),
 ( 0.000000000000000000, 0.002003588478668964865, 0.004007176957337929731, 0.005008971196672411079, 0.006010765436006893295, 0.007012559675341373776, 0.008014353914675855992 ),
 .UNSPECIFIED. ) ;
#7432 = CARTESIAN_POINT ( 'NONE',  ( -37.00000000000000000, -8.017766952966344007, -116.9822330470336453 ) ) ;
#7433 = VECTOR ( 'NONE', #8461, 1000.000000000000114 ) ;
#7434 = CARTESIAN_POINT ( 'NONE',  ( -5.000000000000000888, 6.735557395310443009E-16, 5.000000000000000000 ) ) ;
#7435 = DIRECTION ( 'NONE',  ( -0.7071067811865510144, -0.7071067811865441310, 0.000000000000000000 ) ) ;
#7436 = VERTEX_POINT ( 'NONE', #3369 ) ;
#7437 = EDGE_LOOP ( 'NONE', ( #1276, #8329, #7720, #7969 ) ) ;
#7438 = CARTESIAN_POINT ( 'NONE',  ( -9.137893445389543956, 16.80902845677650603, 30.01486240525018445 ) ) ;
#7439 = EDGE_CURVE ( 'NONE', #7294, #5417, #7555, .T. ) ;
#7440 = CARTESIAN_POINT ( 'NONE',  ( 28.50000000000000355, 7.347880794884123680E-16, 2.000000000000035083 ) ) ;
#7441 = CARTESIAN_POINT ( 'NONE',  ( -2.750000000000002665, -0.7500000000000000000, 1.500000000000000000 ) ) ;
#7442 = DIRECTION ( 'NONE',  ( -1.000000000000000000, 0.000000000000000000, -0.000000000000000000 ) ) ;
#7443 = AXIS2_PLACEMENT_3D ( 'NONE', #6736, #5188, #4424 ) ;
#7444 = EDGE_CURVE ( 'NONE', #9400, #6408, #4092, .T. ) ;
#7445 = DIRECTION ( 'NONE',  ( -1.000000000000000000, 0.000000000000000000, 0.000000000000000000 ) ) ;
#7446 = CARTESIAN_POINT ( 'NONE',  ( 0.000000000000000000, 0.000000000000000000, 22.50000000000000000 ) ) ;
#7447 = CARTESIAN_POINT ( 'NONE',  ( 51.96152422706634155, -29.99999999999996447, -13.00000000000001066 ) ) ;
#7448 = LINE ( 'NONE', #1643, #1271 ) ;
#7449 = ORIENTED_EDGE ( 'NONE', *, *, #907, .T. ) ;
#7450 = ORIENTED_EDGE ( 'NONE', *, *, #6550, .F. ) ;
#7451 = CIRCLE ( 'NONE', #1777, 30.00000000000000000 ) ;
#7452 = PLANE ( 'NONE',  #7713 ) ;
#7453 = FACE_OUTER_BOUND ( 'NONE', #827, .T. ) ;
#7454 = DIRECTION ( 'NONE',  ( 0.6785983445458479979, 0.2810846377148130126, -0.6785983445458491081 ) ) ;
#7455 = CARTESIAN_POINT ( 'NONE',  ( 0.000000000000000000, 17.50000000000000000, 49.50000000000000000 ) ) ;
#7456 = AXIS2_PLACEMENT_3D ( 'NONE', #1896, #4641, #4822 ) ;
#7457 = AXIS2_PLACEMENT_3D ( 'NONE', #5418, #1084, #366 ) ;
#7458 = ORIENTED_EDGE ( 'NONE', *, *, #2998, .T. ) ;
#7459 = PRODUCT_DEFINITION_SHAPE ( 'NONE', 'NONE',  #9487 ) ;
#7460 = ORIENTED_EDGE ( 'NONE', *, *, #6754, .F. ) ;
#7461 = EDGE_LOOP ( 'NONE', ( #977, #8419, #872, #7677 ) ) ;
#7462 = ORIENTED_EDGE ( 'NONE', *, *, #6949, .F. ) ;
#7463 = DIRECTION ( 'NONE',  ( -1.000000000000000000, 0.000000000000000000, 0.000000000000000000 ) ) ;
#7464 = ADVANCED_FACE ( 'NONE', ( #1980 ), #7838, .T. ) ;
#7465 = LINE ( 'NONE', #890, #4275 ) ;
#7466 = EDGE_CURVE ( 'NONE', #3433, #2331, #7698, .T. ) ;
#7467 = LINE ( 'NONE', #2911, #6394 ) ;
#7468 = CIRCLE ( 'NONE', #4863, 2.000000000000000000 ) ;
#7469 = CARTESIAN_POINT ( 'NONE',  ( -16.50000000000000000, 7.347880794884123680E-16, 2.000000000000039080 ) ) ;
#7470 = AXIS2_PLACEMENT_3D ( 'NONE', #3663, #4474, #3036 ) ;
#7471 = DIRECTION ( 'NONE',  ( 1.000000000000000000, 0.000000000000000000, 0.000000000000000000 ) ) ;
#7472 = DIRECTION ( 'NONE',  ( 0.000000000000000000, -0.7071067811865473507, -0.7071067811865477948 ) ) ;
#7473 = VECTOR ( 'NONE', #8367, 1000.000000000000000 ) ;
#7474 = CARTESIAN_POINT ( 'NONE',  ( 5.000000000000000000, 20.00000000000120437, -1.559999999998198161 ) ) ;
#7475 = AXIS2_PLACEMENT_3D ( 'NONE', #5142, #8129, #8024 ) ;
#7476 = EDGE_LOOP ( 'NONE', ( #9, #6977, #3937, #6023, #9089, #4652 ) ) ;
#7477 = VERTEX_POINT ( 'NONE', #1155 ) ;
#7478 = CIRCLE ( 'NONE', #3339, 1.000000000000000888 ) ;
#7479 = DIRECTION ( 'NONE',  ( 1.000000000000000000, 0.000000000000000000, -0.000000000000000000 ) ) ;
#7480 = DIRECTION ( 'NONE',  ( -0.000000000000000000, -0.000000000000000000, 1.000000000000000000 ) ) ;
#7481 = VERTEX_POINT ( 'NONE', #1246 ) ;
#7482 = CARTESIAN_POINT ( 'NONE',  ( 5.373124232108025033, 27.28744256482707087, 0.8097845059602708506 ) ) ;
#7483 = CIRCLE ( 'NONE', #887, 1.560000000000134168 ) ;
#7484 = VECTOR ( 'NONE', #2048, 1000.000000000000000 ) ;
#7485 = CARTESIAN_POINT ( 'NONE',  ( -27.00000000000000000, 43.00000000000000000, 25.00000000000000000 ) ) ;
#7486 = UNCERTAINTY_MEASURE_WITH_UNIT (LENGTH_MEASURE( 1.000000000000000082E-05 ), #3038, 'distance_accuracy_value', 'NONE');
#7487 = CARTESIAN_POINT ( 'NONE',  ( 1.356121383298963590, -28.66577847273270763, 1.695857589613878558 ) ) ;
#7488 = ORIENTED_EDGE ( 'NONE', *, *, #8326, .T. ) ;
#7489 = ORIENTED_EDGE ( 'NONE', *, *, #4066, .F. ) ;
#7490 = APPLICATION_PROTOCOL_DEFINITION ( 'draft international standard', 'automotive_design', 1998, #2480 ) ;
#7491 = DIRECTION ( 'NONE',  ( -1.000000000000000000, 0.000000000000000000, 0.000000000000000000 ) ) ;
#7492 = CIRCLE ( 'NONE', #7041, 7.250000000000002665 ) ;
#7493 = CARTESIAN_POINT ( 'NONE',  ( 53.29490495164537833, 15.90990257669733943, -85.90990257669729147 ) ) ;
#7494 = CIRCLE ( 'NONE', #442, 6.000000000000000888 ) ;
#7495 = PRODUCT_DEFINITION_CONTEXT ( 'detailed design', #996, 'design' ) ;
#7496 = DIRECTION ( 'NONE',  ( 0.000000000000000000, 0.000000000000000000, 1.000000000000000000 ) ) ;
#7497 = ADVANCED_BREP_SHAPE_REPRESENTATION ( '', ( #3184, #1614 ), #3782 ) ;
#7498 = CYLINDRICAL_SURFACE ( 'NONE', #6938, 0.7499999999986606269 ) ;
#7499 = LINE ( 'NONE', #2607, #5816 ) ;
#7500 = DIRECTION ( 'NONE',  ( -1.000000000000000000, 0.000000000000000000, 0.000000000000000000 ) ) ;
#7501 = DIRECTION ( 'NONE',  ( -0.000000000000000000, -0.000000000000000000, -1.000000000000000000 ) ) ;
#7502 = CIRCLE ( 'NONE', #2132, 3.000000000000002665 ) ;
#7503 = ORIENTED_EDGE ( 'NONE', *, *, #8571, .T. ) ;
#7504 = FILL_AREA_STYLE_COLOUR ( '', #3478 ) ;
#7505 = EDGE_LOOP ( 'NONE', ( #229, #1619, #3625, #6725 ) ) ;
#7506 = CARTESIAN_POINT ( 'NONE',  ( -0.7500000000000000000, -0.7500000000000000000, 1.500000000000000000 ) ) ;
#7507 = DIRECTION ( 'NONE',  ( 1.000000000000000000, 0.000000000000000000, 0.000000000000000000 ) ) ;
#7508 = LINE ( 'NONE', #8228, #8119 ) ;
#7509 = DIRECTION ( 'NONE',  ( -1.000000000000000000, -0.000000000000000000, -0.000000000000000000 ) ) ;
#7510 = VERTEX_POINT ( 'NONE', #7108 ) ;
#7511 = ORIENTED_EDGE ( 'NONE', *, *, #3446, .T. ) ;
#7512 = VERTEX_POINT ( 'NONE', #9265 ) ;
#7513 = SHAPE_REPRESENTATION_RELATIONSHIP ( 'NONE' , 'NONE' ,  #7573, #7727 ) ;
#7514 = EDGE_LOOP ( 'NONE', ( #3909, #120 ) ) ;
#7515 = EDGE_CURVE ( 'NONE', #5921, #763, #1882, .T. ) ;
#7516 = DIRECTION ( 'NONE',  ( -1.000000000000000000, 0.000000000000000000, 0.000000000000000000 ) ) ;
#7517 = LINE ( 'NONE', #8240, #3045 ) ;
#7518 =( BOUNDED_CURVE ( )  B_SPLINE_CURVE ( 3, ( #1326, #3304, #9295, #4797 ),
 .UNSPECIFIED., .F., .T. ) 
 B_SPLINE_CURVE_WITH_KNOTS ( ( 4, 4 ),
 ( 1.570796326794896558, 1.948494305174372609 ),
 .UNSPECIFIED. ) 
 CURVE ( )  GEOMETRIC_REPRESENTATION_ITEM ( )  RATIONAL_B_SPLINE_CURVE ( ( 1.000000000000000000, 0.9881473088045071851, 0.9881473088045071851, 1.000000000000000000 ) ) 
 REPRESENTATION_ITEM ( '' )  );
#7519 = CARTESIAN_POINT ( 'NONE',  ( -38.00000000000000711, -43.00000000000000000, 11.99999999999999645 ) ) ;
#7520 = DIRECTION ( 'NONE',  ( 0.000000000000000000, 0.000000000000000000, 1.000000000000000000 ) ) ;
#7521 = CARTESIAN_POINT ( 'NONE',  ( -37.22467645238199196, -47.05659850664387278, 11.99999999999999645 ) ) ;
#7522 = FILL_AREA_STYLE_COLOUR ( '', #4824 ) ;
#7523 = DIRECTION ( 'NONE',  ( -1.000000000000000000, 0.000000000000000000, 0.000000000000000000 ) ) ;
#7524 = VERTEX_POINT ( 'NONE', #527 ) ;
#7525 = EDGE_CURVE ( 'NONE', #4838, #943, #5413, .T. ) ;
#7526 = EDGE_LOOP ( 'NONE', ( #502, #6398, #7129, #8956 ) ) ;
#7527 = CARTESIAN_POINT ( 'NONE',  ( 19.50000000000000355, 0.000000000000000000, 10.00000000000000000 ) ) ;
#7528 = CIRCLE ( 'NONE', #5230, 7.250000000000002665 ) ;
#7529 = EDGE_LOOP ( 'NONE', ( #576, #8788, #3344, #5656, #4758 ) ) ;
#7530 = EDGE_CURVE ( 'NONE', #5683, #5609, #3106, .T. ) ;
#7531 = DIRECTION ( 'NONE',  ( 0.000000000000000000, 0.000000000000000000, 1.000000000000000000 ) ) ;
#7532 = CARTESIAN_POINT ( 'NONE',  ( 22.50000000000000355, 2.356749903719115078E-13, 5.000000000000000000 ) ) ;
#7533 = ADVANCED_FACE ( 'NONE', ( #4048 ), #798, .F. ) ;
#7534 = ADVANCED_FACE ( 'NONE', ( #7793 ), #2658, .F. ) ;
#7535 = VERTEX_POINT ( 'NONE', #6353 ) ;
#7536 = CARTESIAN_POINT ( 'NONE',  ( -37.00000000000000711, 15.90990257669733943, -54.09009742330271564 ) ) ;
#7537 = AXIS2_PLACEMENT_3D ( 'NONE', #5651, #8525, #1309 ) ;
#7538 = DIRECTION ( 'NONE',  ( -1.000000000000000000, 0.000000000000000000, 0.000000000000000000 ) ) ;
#7539 = CARTESIAN_POINT ( 'NONE',  ( -0.6691251631324991456, -28.75033890800110825, 1.750217869429287365 ) ) ;
#7540 = ORIENTED_EDGE ( 'NONE', *, *, #1824, .T. ) ;
#7541 = VERTEX_POINT ( 'NONE', #390 ) ;
#7542 = CARTESIAN_POINT ( 'NONE',  ( 0.000000000000000000, 0.000000000000000000, 0.000000000000000000 ) ) ;
#7543 = EDGE_CURVE ( 'NONE', #4790, #4735, #3320, .T. ) ;
#7544 = CYLINDRICAL_SURFACE ( 'NONE', #2858, 0.7500000000012114754 ) ;
#7545 = EDGE_CURVE ( 'NONE', #9313, #4476, #3874, .T. ) ;
#7546 = CARTESIAN_POINT ( 'NONE',  ( -43.18827341296429267, -42.33902489539480030, -7.653089211995582453 ) ) ;
#7547 = FACE_OUTER_BOUND ( 'NONE', #8904, .T. ) ;
#7548 = DIRECTION ( 'NONE',  ( 0.000000000000000000, 0.000000000000000000, 1.000000000000000000 ) ) ;
#7549 = DIRECTION ( 'NONE',  ( 0.000000000000000000, 0.000000000000000000, 1.000000000000000000 ) ) ;
#7550 = VERTEX_POINT ( 'NONE', #722 ) ;
#7551 = CARTESIAN_POINT ( 'NONE',  ( -37.00000000000000711, 15.90990257669733943, -85.90990257669729147 ) ) ;
#7552 = ORIENTED_EDGE ( 'NONE', *, *, #6131, .T. ) ;
#7553 = PLANE ( 'NONE',  #6951 ) ;
#7554 = DIRECTION ( 'NONE',  ( -1.000000000000000000, 0.000000000000000000, 0.000000000000000000 ) ) ;
#7555 = CIRCLE ( 'NONE', #2036, 60.00000000000000000 ) ;
#7556 = CARTESIAN_POINT ( 'NONE',  ( 0.000000000000000000, 0.000000000000000000, 4.000000000000000000 ) ) ;
#7557 = CARTESIAN_POINT ( 'NONE',  ( 19.50000000000000355, 2.356749903719115078E-13, 10.00000000000000000 ) ) ;
#7558 = ORIENTED_EDGE ( 'NONE', *, *, #228, .F. ) ;
#7559 = ORIENTED_EDGE ( 'NONE', *, *, #3413, .T. ) ;
#7560 = ORIENTED_EDGE ( 'NONE', *, *, #6961, .F. ) ;
#7561 = EDGE_LOOP ( 'NONE', ( #4036, #6679 ) ) ;
#7562 = DIRECTION ( 'NONE',  ( 1.000000000000000000, -0.000000000000000000, -0.000000000000000000 ) ) ;
#7563 = DIRECTION ( 'NONE',  ( 1.000000000000000000, 0.000000000000000000, 0.000000000000000000 ) ) ;
#7564 = CARTESIAN_POINT ( 'NONE',  ( 1.749999999999985345, -1.750000000000001554, 0.000000000000000000 ) ) ;
#7565 = EDGE_CURVE ( 'NONE', #5946, #5859, #5190, .T. ) ;
#7566 = CARTESIAN_POINT ( 'NONE',  ( 27.00000000000000000, 43.00000000000000000, 11.99999999999999645 ) ) ;
#7567 = CARTESIAN_POINT ( 'NONE',  ( 0.000000000000000000, 0.000000000000000000, 20.49999999999999645 ) ) ;
#7568 = VECTOR ( 'NONE', #5905, 1000.000000000000000 ) ;
#7569 = CARTESIAN_POINT ( 'NONE',  ( -30.00000000000000000, 0.000000000000000000, 10.00000000000000000 ) ) ;
#7570 = CYLINDRICAL_SURFACE ( 'NONE', #6970, 3.000000000000000000 ) ;
#7571 = ORIENTED_EDGE ( 'NONE', *, *, #3843, .F. ) ;
#7572 = ORIENTED_EDGE ( 'NONE', *, *, #8529, .F. ) ;
#7573 = SHAPE_REPRESENTATION ( '3-Flange Yoke', ( #1614 ), #6101 ) ;
#7574 = CARTESIAN_POINT ( 'NONE',  ( 19.00000000000000000, 0.000000000000000000, 0.000000000000000000 ) ) ;
#7575 = EDGE_LOOP ( 'NONE', ( #6774, #4878 ) ) ;
#7576 = PLANE ( 'NONE',  #7337 ) ;
#7577 = CARTESIAN_POINT ( 'NONE',  ( -12.37436867076458036, 12.37436867076458036, 44.37436867076458213 ) ) ;
#7578 = VERTEX_POINT ( 'NONE', #7980 ) ;
#7579 = FACE_OUTER_BOUND ( 'NONE', #3237, .T. ) ;
#7580 = EDGE_CURVE ( 'NONE', #5050, #754, #5141, .T. ) ;
#7581 = AXIS2_PLACEMENT_3D ( 'NONE', #2545, #8348, #4704 ) ;
#7582 = FACE_BOUND ( 'NONE', #53, .T. ) ;
#7583 = CYLINDRICAL_SURFACE ( 'NONE', #2102, 11.00000000000000000 ) ;
#7584 = ORIENTED_EDGE ( 'NONE', *, *, #6234, .T. ) ;
#7585 = VERTEX_POINT ( 'NONE', #6594 ) ;
#7586 = CIRCLE ( 'NONE', #8045, 15.66147716702868209 ) ;
#7587 = CARTESIAN_POINT ( 'NONE',  ( 5.000000000000000000, 7.653668647300657213, -18.47759065022568237 ) ) ;
#7588 = CARTESIAN_POINT ( 'NONE',  ( 17.50000000000000355, 0.000000000000000000, 49.50000000000000000 ) ) ;
#7589 = EDGE_CURVE ( 'NONE', #8372, #5946, #1629, .T. ) ;
#7590 = VECTOR ( 'NONE', #6393, 1000.000000000000000 ) ;
#7591 = DIRECTION ( 'NONE',  ( 0.000000000000000000, 0.000000000000000000, -1.000000000000000000 ) ) ;
#7592 = SURFACE_STYLE_USAGE ( .BOTH. , #6835 ) ;
#7593 = FACE_OUTER_BOUND ( 'NONE', #5633, .T. ) ;
#7594 = EDGE_CURVE ( 'NONE', #8767, #2584, #3747, .T. ) ;
#7595 = PLANE ( 'NONE',  #2671 ) ;
#7596 = VERTEX_POINT ( 'NONE', #8696 ) ;
#7597 = ORIENTED_EDGE ( 'NONE', *, *, #1517, .F. ) ;
#7598 = DIRECTION ( 'NONE',  ( -0.000000000000000000, -0.000000000000000000, 1.000000000000000000 ) ) ;
#7599 = DIRECTION ( 'NONE',  ( -1.000000000000000000, -0.000000000000000000, -0.000000000000000000 ) ) ;
#7600 = AXIS2_PLACEMENT_3D ( 'NONE', #4057, #3329, #7295 ) ;
#7601 = FACE_OUTER_BOUND ( 'NONE', #6899, .T. ) ;
#7602 = CYLINDRICAL_SURFACE ( 'NONE', #189, 1.560000000000000719 ) ;
#7603 = VERTEX_POINT ( 'NONE', #6541 ) ;
#7604 = ORIENTED_EDGE ( 'NONE', *, *, #368, .F. ) ;
#7605 = CIRCLE ( 'NONE', #6692, 5.000000000000000888 ) ;
#7606 = ORIENTED_EDGE ( 'NONE', *, *, #8695, .T. ) ;
#7607 =( NAMED_UNIT ( * ) PLANE_ANGLE_UNIT ( ) SI_UNIT ( $, .RADIAN. ) );
#7608 = EDGE_LOOP ( 'NONE', ( #412, #1936, #885, #9206 ) ) ;
#7609 = CARTESIAN_POINT ( 'NONE',  ( -28.50000000000001066, -0.2131062308234238922, 1.500000000000038858 ) ) ;
#7610 = DIRECTION ( 'NONE',  ( 0.000000000000000000, 0.000000000000000000, -1.000000000000000000 ) ) ;
#7611 = DIRECTION ( 'NONE',  ( 0.000000000000000000, 0.000000000000000000, -1.000000000000000000 ) ) ;
#7612 = DIRECTION ( 'NONE',  ( 0.000000000000000000, 0.000000000000000000, 1.000000000000000000 ) ) ;
#7613 = CARTESIAN_POINT ( 'NONE',  ( -6.000000000000000888, 22.50000000000000355, 0.000000000000000000 ) ) ;
#7614 = DIRECTION ( 'NONE',  ( -1.000000000000000000, 0.000000000000000000, 0.000000000000000000 ) ) ;
#7615 = EDGE_CURVE ( 'NONE', #5090, #3120, #7914, .T. ) ;
#7616 = ORIENTED_EDGE ( 'NONE', *, *, #4535, .T. ) ;
#7617 = ORIENTED_EDGE ( 'NONE', *, *, #5113, .T. ) ;
#7618 = EDGE_CURVE ( 'NONE', #1857, #720, #5053, .T. ) ;
#7619 = DIRECTION ( 'NONE',  ( 0.000000000000000000, 0.7071067811865479058, -0.7071067811865472397 ) ) ;
#7620 = ORIENTED_EDGE ( 'NONE', *, *, #9320, .T. ) ;
#7621 = ADVANCED_FACE ( 'NONE', ( #2976 ), #4329, .F. ) ;
#7622 = AXIS2_PLACEMENT_3D ( 'NONE', #1650, #8371, #348 ) ;
#7623 = CARTESIAN_POINT ( 'NONE',  ( -4.119968255444916849E-15, -3.500000000000000000, 1.500000000000000000 ) ) ;
#7624 = CARTESIAN_POINT ( 'NONE',  ( 60.00000000000000000, 15.90990257669733943, -54.09009742330271564 ) ) ;
#7625 = ORIENTED_EDGE ( 'NONE', *, *, #1833, .T. ) ;
#7626 = EDGE_CURVE ( 'NONE', #7535, #4745, #6090, .T. ) ;
#7627 = DIRECTION ( 'NONE',  ( -0.7071067811865441310, 0.7071067811865510144, -0.000000000000000000 ) ) ;
#7628 = CIRCLE ( 'NONE', #2875, 1.000000000000000000 ) ;
#7629 = AXIS2_PLACEMENT_3D ( 'NONE', #706, #5225, #2196 ) ;
#7630 = DIRECTION ( 'NONE',  ( -1.000000000000000000, 0.000000000000000000, 0.000000000000000000 ) ) ;
#7631 = CARTESIAN_POINT ( 'NONE',  ( 3.299340129088522922, -28.21697752735853726, 1.407342696159064488 ) ) ;
#7632 = CIRCLE ( 'NONE', #1648, 1.560000000002236709 ) ;
#7633 = EDGE_LOOP ( 'NONE', ( #8509, #9423, #7262, #6102 ) ) ;
#7634 = EDGE_LOOP ( 'NONE', ( #2129, #293, #5826 ) ) ;
#7635 = VECTOR ( 'NONE', #4455, 1000.000000000000114 ) ;
#7636 = APPLICATION_PROTOCOL_DEFINITION ( 'draft international standard', 'automotive_design', 1998, #4617 ) ;
#7637 = AXIS2_PLACEMENT_3D ( 'NONE', #142, #5853, #3066 ) ;
#7638 = EDGE_CURVE ( 'NONE', #5792, #9435, #5472, .T. ) ;
#7639 = AXIS2_PLACEMENT_3D ( 'NONE', #8269, #915, #3892 ) ;
#7640 = PLANE ( 'NONE',  #4266 ) ;
#7641 = VECTOR ( 'NONE', #4028, 1000.000000000000000 ) ;
#7642 = CARTESIAN_POINT ( 'NONE',  ( -31.99999999999999289, 0.000000000000000000, 14.49999999999999467 ) ) ;
#7643 = CARTESIAN_POINT ( 'NONE',  ( -19.74999999999999645, 43.00000000000000000, 11.99999999999999645 ) ) ;
#7644 = DIRECTION ( 'NONE',  ( -1.000000000000000000, -0.000000000000000000, -0.000000000000000000 ) ) ;
#7645 = CARTESIAN_POINT ( 'NONE',  ( -28.11123945536280644, 3.602653646940651377, 1.339368221304670037 ) ) ;
#7646 = ADVANCED_FACE ( 'NONE', ( #8128 ), #2261, .T. ) ;
#7647 = ORIENTED_EDGE ( 'NONE', *, *, #7908, .F. ) ;
#7648 = ADVANCED_FACE ( 'NONE', ( #2208 ), #6681, .F. ) ;
#7649 = DIRECTION ( 'NONE',  ( -1.000000000000000000, 0.000000000000000000, 0.000000000000000000 ) ) ;
#7650 = AXIS2_PLACEMENT_3D ( 'NONE', #3099, #8725, #6705 ) ;
#7651 = VERTEX_POINT ( 'NONE', #3698 ) ;
#7652 = CIRCLE ( 'NONE', #2279, 15.00000000000000000 ) ;
#7653 = DIRECTION ( 'NONE',  ( -1.000000000000000000, 0.000000000000000000, 0.000000000000000000 ) ) ;
#7654 = EDGE_CURVE ( 'NONE', #2690, #5694, #9462, .T. ) ;
#7655 = CARTESIAN_POINT ( 'NONE',  ( 0.000000000000000000, 0.000000000000000000, 10.00000000000000000 ) ) ;
#7656 = CARTESIAN_POINT ( 'NONE',  ( -37.00000000000000711, -15.90990257669733943, -51.09009742330271564 ) ) ;
#7657 = CARTESIAN_POINT ( 'NONE',  ( 51.96152422706634155, -29.99999999999996447, -13.00000000000001066 ) ) ;
#7658 = CIRCLE ( 'NONE', #8878, 11.00000000000000000 ) ;
#7659 = CIRCLE ( 'NONE', #3507, 6.000000000000000888 ) ;
#7660 = ORIENTED_EDGE ( 'NONE', *, *, #8140, .F. ) ;
#7661 = EDGE_LOOP ( 'NONE', ( #4968, #7248, #4698, #6204, #944, #8553 ) ) ;
#7662 = ORIENTED_EDGE ( 'NONE', *, *, #8071, .T. ) ;
#7663 =( LENGTH_UNIT ( ) NAMED_UNIT ( * ) SI_UNIT ( .MILLI., .METRE. ) );
#7664 = ORIENTED_EDGE ( 'NONE', *, *, #8177, .F. ) ;
#7665 = EDGE_CURVE ( 'NONE', #6124, #4363, #3774, .T. ) ;
#7666 = CARTESIAN_POINT ( 'NONE',  ( 49.75937104571250558, -12.92893218813459910, -101.0355339059328657 ) ) ;
#7667 = EDGE_CURVE ( 'NONE', #1699, #2294, #8745, .T. ) ;
#7668 = CARTESIAN_POINT ( 'NONE',  ( -39.50000000000000711, -30.00000000000000355, -82.50000000000001421 ) ) ;
#7669 = EDGE_CURVE ( 'NONE', #720, #6525, #7693, .T. ) ;
#7670 = LINE ( 'NONE', #9055, #937 ) ;
#7671 = DIRECTION ( 'NONE',  ( 0.000000000000000000, 0.000000000000000000, 1.000000000000000000 ) ) ;
#7672 = CARTESIAN_POINT ( 'NONE',  ( 28.75000000000001776, 7.654042494438380704E-16, 1.750000000000019762 ) ) ;
#7673 = ORIENTED_EDGE ( 'NONE', *, *, #3608, .F. ) ;
#7674 = VERTEX_POINT ( 'NONE', #6012 ) ;
#7675 = AXIS2_PLACEMENT_3D ( 'NONE', #392, #4629, #8428 ) ;
#7676 = DIRECTION ( 'NONE',  ( -1.000000000000000000, 0.000000000000000000, 0.000000000000000000 ) ) ;
#7677 = ORIENTED_EDGE ( 'NONE', *, *, #8369, .F. ) ;
#7678 = FACE_BOUND ( 'NONE', #6603, .T. ) ;
#7679 = DIRECTION ( 'NONE',  ( 1.000000000000000000, 0.000000000000000000, 0.000000000000000000 ) ) ;
#7680 = ORIENTED_EDGE ( 'NONE', *, *, #731, .T. ) ;
#7681 = CARTESIAN_POINT ( 'NONE',  ( 16.00000000000000000, 0.000000000000000000, 11.00000000000000000 ) ) ;
#7682 = DIRECTION ( 'NONE',  ( -1.000000000000000000, 0.000000000000000000, 0.000000000000000000 ) ) ;
#7683 = CIRCLE ( 'NONE', #323, 0.7499999999982936982 ) ;
#7684 = CARTESIAN_POINT ( 'NONE',  ( 27.00000000000000000, -43.00000000000000000, 11.99999999999999645 ) ) ;
#7685 = VERTEX_POINT ( 'NONE', #6296 ) ;
#7686 = ORIENTED_EDGE ( 'NONE', *, *, #8947, .F. ) ;
#7687 = ITEM_DEFINED_TRANSFORMATION ( 'NONE', 'NONE', #3919,  #1614 ) ;
#7688 = ADVANCED_FACE ( 'NONE', ( #245 ), #7544, .F. ) ;
#7689 = VECTOR ( 'NONE', #6418, 1000.000000000000000 ) ;
#7690 = LINE ( 'NONE', #3995, #2105 ) ;
#7691 = CARTESIAN_POINT ( 'NONE',  ( 9.048619709455111959, 15.70011763207404876, 47.70011763207404698 ) ) ;
#7692 = DIRECTION ( 'NONE',  ( -1.000000000000000000, 0.000000000000000000, 0.000000000000000000 ) ) ;
#7693 = B_SPLINE_CURVE_WITH_KNOTS ( 'NONE', 3,
 ( #5963, #4997, #2162, #7928, #1346, #4285, #3557, #6498, #8023, #1439, #9027, #3794 ),
 .UNSPECIFIED., .F., .F.,
 ( 4, 2, 2, 2, 2, 4 ),
 ( 0.005117570262457546253, 0.006390849577664815817, 0.007027489235268451033, 0.007664128892872086249, 0.008937408208079361885, 0.01021068752328663752 ),
 .UNSPECIFIED. ) ;
#7694 = CARTESIAN_POINT ( 'NONE',  ( -28.75000000000002132, 2.329604860730800488E-26, 1.750000000000023537 ) ) ;
#7695 = EDGE_LOOP ( 'NONE', ( #4179, #5430, #1105, #9128 ) ) ;
#7696 = CYLINDRICAL_SURFACE ( 'NONE', #1333, 1.559999999999096776 ) ;
#7697 = VERTEX_POINT ( 'NONE', #5289 ) ;
#7698 = LINE ( 'NONE', #7158, #2345 ) ;
#7699 = AXIS2_PLACEMENT_3D ( 'NONE', #1159, #8429, #3373 ) ;
#7700 = CARTESIAN_POINT ( 'NONE',  ( -37.00000000000000711, -3.673940397442057600E-15, -70.00000000000000000 ) ) ;
#7701 = DIRECTION ( 'NONE',  ( -1.000000000000000000, 0.000000000000000000, 0.000000000000000000 ) ) ;
#7702 = EDGE_CURVE ( 'NONE', #1434, #2697, #7605, .T. ) ;
#7703 = CARTESIAN_POINT ( 'NONE',  ( -26.99999999999996092, 35.00000000000000000, 0.000000000000000000 ) ) ;
#7704 = EDGE_CURVE ( 'NONE', #3516, #6408, #7451, .T. ) ;
#7705 = ADVANCED_FACE ( 'NONE', ( #2639 ), #5571, .F. ) ;
#7706 = EDGE_CURVE ( 'NONE', #1656, #4910, #4085, .T. ) ;
#7707 = CIRCLE ( 'NONE', #5092, 3.000000000000000000 ) ;
#7708 = ORIENTED_EDGE ( 'NONE', *, *, #5228, .T. ) ;
#7709 = VERTEX_POINT ( 'NONE', #3846 ) ;
#7710 = CARTESIAN_POINT ( 'NONE',  ( 7.219041098785725197, 143.7302683746874550, 42.45188461190927143 ) ) ;
#7711 = ORIENTED_EDGE ( 'NONE', *, *, #5990, .T. ) ;
#7712 = CARTESIAN_POINT ( 'NONE',  ( 4.703319286132082055, -17.49999999999999645, 14.50000000000000178 ) ) ;
#7713 = AXIS2_PLACEMENT_3D ( 'NONE', #8318, #6841, #8989 ) ;
#7714 = LINE ( 'NONE', #5556, #710 ) ;
#7715 = LINE ( 'NONE', #1080, #5077 ) ;
#7716 = CARTESIAN_POINT ( 'NONE',  ( 27.00000000000000355, -34.99999999999999289, 5.000000000000004441 ) ) ;
#7717 = TOROIDAL_SURFACE ( 'NONE', #3568, 13.50000000000000178, 1.000000000000000000 ) ;
#7718 = DIRECTION ( 'NONE',  ( -0.000000000000000000, -0.000000000000000000, -1.000000000000000000 ) ) ;
#7719 = EDGE_LOOP ( 'NONE', ( #2447, #2696, #7212, #2431, #3575, #6504 ) ) ;
#7720 = ORIENTED_EDGE ( 'NONE', *, *, #2186, .T. ) ;
#7721 = CARTESIAN_POINT ( 'NONE',  ( -37.00000000000000000, -21.98223304703364889, -86.98223304703364533 ) ) ;
#7722 = ORIENTED_EDGE ( 'NONE', *, *, #3139, .F. ) ;
#7723 = ADVANCED_FACE ( 'NONE', ( #2312 ), #859, .F. ) ;
#7724 = CARTESIAN_POINT ( 'NONE',  ( 53.29490495164537833, -30.00000000000000000, -41.61356529332876875 ) ) ;
#7725 = DIRECTION ( 'NONE',  ( 0.000000000000000000, 0.000000000000000000, 1.000000000000000000 ) ) ;
#7726 = ORIENTED_EDGE ( 'NONE', *, *, #774, .F. ) ;
#7727 = ADVANCED_BREP_SHAPE_REPRESENTATION ( '', ( #6348, #1614 ), #6101 ) ;
#7728 = DIRECTION ( 'NONE',  ( 0.000000000000000000, -1.000000000000000000, 0.000000000000000000 ) ) ;
#7729 = AXIS2_PLACEMENT_3D ( 'NONE', #2693, #2062, #8688 ) ;
#7730 = ADVANCED_FACE ( 'NONE', ( #201, #4122 ), #4839, .T. ) ;
#7731 = CARTESIAN_POINT ( 'NONE',  ( -22.50000000000000355, 0.000000000000000000, 5.000000000000000000 ) ) ;
#7732 = DIRECTION ( 'NONE',  ( 1.000000000000000000, -0.000000000000000000, -0.000000000000000000 ) ) ;
#7733 = VERTEX_POINT ( 'NONE', #8169 ) ;
#7734 = ORIENTED_EDGE ( 'NONE', *, *, #2543, .T. ) ;
#7735 = VECTOR ( 'NONE', #2675, 1000.000000000000000 ) ;
#7736 = CONTEXT_DEPENDENT_SHAPE_REPRESENTATION ( #3631, #5779 ) ;
#7737 = DIRECTION ( 'NONE',  ( -1.000000000000000000, 0.000000000000000000, 0.000000000000000000 ) ) ;
#7738 = CARTESIAN_POINT ( 'NONE',  ( -22.50000000000000355, 0.000000000000000000, 10.00000000000000000 ) ) ;
#7739 = DIRECTION ( 'NONE',  ( -1.000000000000000000, 0.000000000000000000, 0.000000000000000000 ) ) ;
#7740 = FACE_OUTER_BOUND ( 'NONE', #9019, .T. ) ;
#7741 = EDGE_CURVE ( 'NONE', #6082, #7367, #8076, .T. ) ;
#7742 = VERTEX_POINT ( 'NONE', #3351 ) ;
#7743 = CIRCLE ( 'NONE', #9421, 0.7499999999986606269 ) ;
#7744 = ORIENTED_EDGE ( 'NONE', *, *, #9399, .F. ) ;
#7745 = DIRECTION ( 'NONE',  ( 0.000000000000000000, -0.000000000000000000, -1.000000000000000000 ) ) ;
#7746 = TOROIDAL_SURFACE ( 'NONE', #828, 16.00000000000000000, 1.000000000000000000 ) ;
#7747 = CARTESIAN_POINT ( 'NONE',  ( -50.79490495164537833, -30.00000000000000000, -100.0000000000000000 ) ) ;
#7748 = ADVANCED_FACE ( 'NONE', ( #6782 ), #4614, .F. ) ;
#7749 = FACE_OUTER_BOUND ( 'NONE', #8955, .T. ) ;
#7750 = CARTESIAN_POINT ( 'NONE',  ( 0.000000000000000000, 0.000000000000000000, 0.000000000000000000 ) ) ;
#7751 = CARTESIAN_POINT ( 'NONE',  ( -8.000000000000021316, -22.50000000000000355, 0.000000000000000000 ) ) ;
#7752 = ORIENTED_EDGE ( 'NONE', *, *, #56, .F. ) ;
#7753 = EDGE_LOOP ( 'NONE', ( #320, #784, #5852, #7427 ) ) ;
#7754 = DIRECTION ( 'NONE',  ( 0.000000000000000000, -0.7071067811865483499, 0.7071067811865467956 ) ) ;
#7755 = ORIENTED_EDGE ( 'NONE', *, *, #2053, .T. ) ;
#7756 = PLANE ( 'NONE',  #6344 ) ;
#7757 = CARTESIAN_POINT ( 'NONE',  ( 0.000000000000000000, -18.47759065022790637, -7.653668647299759265 ) ) ;
#7758 = CARTESIAN_POINT ( 'NONE',  ( 4.000000000000000000, 18.47759065022658120, 8.403668647301545391 ) ) ;
#7759 = CARTESIAN_POINT ( 'NONE',  ( 0.7500000000000000000, -0.7500000000000000000, 1.500000000000000000 ) ) ;
#7760 = AXIS2_PLACEMENT_3D ( 'NONE', #7438, #8267, #8787 ) ;
#7761 = CARTESIAN_POINT ( 'NONE',  ( 4.119968255444916849E-15, 3.500000000000000000, 0.000000000000000000 ) ) ;
#7762 = PRODUCT_DEFINITION ( 'UNKNOWN', '', #8067, #2307 ) ;
#7763 = ORIENTED_EDGE ( 'NONE', *, *, #3712, .F. ) ;
#7764 = EDGE_CURVE ( 'NONE', #6538, #8325, #2361, .T. ) ;
#7765 = EDGE_LOOP ( 'NONE', ( #8752, #7379, #2657, #9432, #6292, #7711, #376, #8018, #1447, #6756, #4214, #1353, #3161, #5984 ) ) ;
#7766 = CARTESIAN_POINT ( 'NONE',  ( -40.00000000000000000, 30.00000000000000000, -13.00000000000000533 ) ) ;
#7767 = ORIENTED_EDGE ( 'NONE', *, *, #8140, .T. ) ;
#7768 = EDGE_CURVE ( 'NONE', #3765, #1975, #4513, .T. ) ;
#7769 = CARTESIAN_POINT ( 'NONE',  ( 60.00000000000000000, -3.673940397442057600E-15, -55.00000000000000711 ) ) ;
#7770 = CARTESIAN_POINT ( 'NONE',  ( -22.50000000000000000, -7.855833012397050680E-14, 5.000000000000000000 ) ) ;
#7771 = ORIENTED_EDGE ( 'NONE', *, *, #3123, .F. ) ;
#7772 = DIRECTION ( 'NONE',  ( 1.000000000000000000, 0.000000000000000000, 0.000000000000000000 ) ) ;
#7773 = CARTESIAN_POINT ( 'NONE',  ( 9.364477336218621772, -62.15368297487813010, 0.9332626224471951559 ) ) ;
#7774 = LINE ( 'NONE', #8542, #518 ) ;
#7775 = CARTESIAN_POINT ( 'NONE',  ( 37.00000000000000000, -30.00000000000000000, -95.00000000000000000 ) ) ;
#7776 = CIRCLE ( 'NONE', #1944, 0.7499999999986606269 ) ;
#7777 = ORIENTED_EDGE ( 'NONE', *, *, #8326, .F. ) ;
#7778 = COLOUR_RGB ( '',0.7921568627450980005, 0.8196078431372548767, 0.9333333333333333481 ) ;
#7779 = ORIENTED_EDGE ( 'NONE', *, *, #847, .F. ) ;
#7780 = LINE ( 'NONE', #1096, #7172 ) ;
#7781 = AXIS2_PLACEMENT_3D ( 'NONE', #8087, #3670, #7361 ) ;
#7782 = CARTESIAN_POINT ( 'NONE',  ( 0.000000000000000000, 0.000000000000000000, 1.500000000000000000 ) ) ;
#7783 = VECTOR ( 'NONE', #1300, 1000.000000000000000 ) ;
#7784 = CARTESIAN_POINT ( 'NONE',  ( 26.64999999999992752, 4.333301281933056970, 0.000000000000000000 ) ) ;
#7785 = PLANE ( 'NONE',  #3946 ) ;
#7786 = AXIS2_PLACEMENT_3D ( 'NONE', #9453, #6733, #2970 ) ;
#7787 = EDGE_LOOP ( 'NONE', ( #3388, #6295, #4227, #2679 ) ) ;
#7788 =( GEOMETRIC_REPRESENTATION_CONTEXT ( 3 ) GLOBAL_UNCERTAINTY_ASSIGNED_CONTEXT ( ( #4419 ) ) GLOBAL_UNIT_ASSIGNED_CONTEXT ( ( #1594, #210, #4674 ) ) REPRESENTATION_CONTEXT ( 'NONE', 'WORKASPACE' ) );
#7789 = VERTEX_POINT ( 'NONE', #5390 ) ;
#7790 = AXIS2_PLACEMENT_3D ( 'NONE', #7493, #961, #6115 ) ;
#7791 = ORIENTED_EDGE ( 'NONE', *, *, #5948, .T. ) ;
#7792 = CONICAL_SURFACE ( 'NONE', #2878, 28.00000000000000711, 0.7853981633974473908 ) ;
#7793 = FACE_OUTER_BOUND ( 'NONE', #6939, .T. ) ;
#7794 = DIRECTION ( 'NONE',  ( 0.000000000000000000, 0.000000000000000000, -1.000000000000000000 ) ) ;
#7795 = DIRECTION ( 'NONE',  ( 0.000000000000000000, 0.000000000000000000, 1.000000000000000000 ) ) ;
#7796 = DIRECTION ( 'NONE',  ( 1.000000000000000000, 0.000000000000000000, 0.000000000000000000 ) ) ;
#7797 = CYLINDRICAL_SURFACE ( 'NONE', #679, 0.7500000000001915135 ) ;
#7798 = COLOUR_RGB ( '',0.7921568627450980005, 0.8196078431372548767, 0.9333333333333333481 ) ;
#7799 = ORIENTED_EDGE ( 'NONE', *, *, #1359, .F. ) ;
#7800 = ORIENTED_EDGE ( 'NONE', *, *, #1576, .T. ) ;
#7801 = DIRECTION ( 'NONE',  ( -6.765421556309547668E-17, 0.9997175446104180629, -0.02376617340079582863 ) ) ;
#7802 = ORIENTED_EDGE ( 'NONE', *, *, #9052, .T. ) ;
#7803 = DIRECTION ( 'NONE',  ( 0.000000000000000000, 0.000000000000000000, 1.000000000000000000 ) ) ;
#7804 = CARTESIAN_POINT ( 'NONE',  ( -27.61492299646193871, 3.160432959937508723, 0.7930775300198876776 ) ) ;
#7805 = CIRCLE ( 'NONE', #7185, 7.250000000000002665 ) ;
#7806 = LINE ( 'NONE', #3521, #5547 ) ;
#7807 = AXIS2_PLACEMENT_3D ( 'NONE', #780, #3672, #1453 ) ;
#7808 = FACE_OUTER_BOUND ( 'NONE', #1386, .T. ) ;
#7809 = LINE ( 'NONE', #406, #8646 ) ;
#7810 = EDGE_CURVE ( 'NONE', #2280, #7970, #8309, .T. ) ;
#7811 = ORIENTED_EDGE ( 'NONE', *, *, #325, .F. ) ;
#7812 = ORIENTED_EDGE ( 'NONE', *, *, #7296, .F. ) ;
#7813 = CARTESIAN_POINT ( 'NONE',  ( 0.000000000000000000, 0.000000000000000000, 27.50000000000000355 ) ) ;
#7814 = AXIS2_PLACEMENT_3D ( 'NONE', #4718, #6975, #207 ) ;
#7815 = VERTEX_POINT ( 'NONE', #7440 ) ;
#7816 = LINE ( 'NONE', #8001, #6895 ) ;
#7817 = DIRECTION ( 'NONE',  ( 1.000000000000000000, -0.000000000000000000, -0.000000000000000000 ) ) ;
#7818 = CARTESIAN_POINT ( 'NONE',  ( 0.000000000000000000, 0.000000000000000000, 10.00000000000000000 ) ) ;
#7819 = CARTESIAN_POINT ( 'NONE',  ( 27.00000000000000000, -43.00000000000000000, -25.00000000000000000 ) ) ;
#7820 = ADVANCED_FACE ( 'NONE', ( #1137 ), #7054, .T. ) ;
#7821 = LINE ( 'NONE', #6435, #1438 ) ;
#7822 = DIRECTION ( 'NONE',  ( -0.7071067811865481278, 0.000000000000000000, -0.7071067811865470176 ) ) ;
#7823 = EDGE_CURVE ( 'NONE', #367, #2399, #6543, .T. ) ;
#7824 = ORIENTED_EDGE ( 'NONE', *, *, #4414, .F. ) ;
#7825 = ORIENTED_EDGE ( 'NONE', *, *, #6665, .F. ) ;
#7826 = EDGE_CURVE ( 'NONE', #1835, #5764, #6243, .T. ) ;
#7827 = EDGE_CURVE ( 'NONE', #5323, #9400, #2050, .T. ) ;
#7828 = ITEM_DEFINED_TRANSFORMATION ( 'NONE', 'NONE', #8825,  #1614 ) ;
#7829 = LINE ( 'NONE', #1147, #7590 ) ;
#7830 = CARTESIAN_POINT ( 'NONE',  ( 4.119968255444916849E-15, 3.500000000000000000, 1.500000000000000000 ) ) ;
#7831 = DIRECTION ( 'NONE',  ( -1.000000000000000000, 0.000000000000000000, -0.000000000000000000 ) ) ;
#7832 = ORIENTED_EDGE ( 'NONE', *, *, #6595, .T. ) ;
#7833 = ORIENTED_EDGE ( 'NONE', *, *, #4636, .T. ) ;
#7834 = ORIENTED_EDGE ( 'NONE', *, *, #6, .T. ) ;
#7835 = VECTOR ( 'NONE', #7863, 1000.000000000000000 ) ;
#7836 = EDGE_LOOP ( 'NONE', ( #2460, #2204, #8692, #7848 ) ) ;
#7837 = EDGE_CURVE ( 'NONE', #5476, #5740, #2709, .T. ) ;
#7838 = PLANE ( 'NONE',  #6028 ) ;
#7839 = CARTESIAN_POINT ( 'NONE',  ( 39.50000000000000000, -30.00000000000000355, -82.50000000000001421 ) ) ;
#7840 = CARTESIAN_POINT ( 'NONE',  ( -11.96410161513786008, 0.000000000000000000, 50.00000000000000000 ) ) ;
#7841 = PRODUCT_DEFINITION_SHAPE ( 'NONE', 'NONE',  #6069 ) ;
#7842 = ADVANCED_FACE ( 'NONE', ( #9347 ), #5030, .F. ) ;
#7843 = CARTESIAN_POINT ( 'NONE',  ( -31.99999999999999289, 0.000000000000000000, 50.50000000000001421 ) ) ;
#7844 = FACE_BOUND ( 'NONE', #2656, .T. ) ;
#7845 = VERTEX_POINT ( 'NONE', #8676 ) ;
#7846 = DIRECTION ( 'NONE',  ( -0.5773502691896235106, -0.000000000000000000, -0.8164965809277276998 ) ) ;
#7847 = DIRECTION ( 'NONE',  ( 0.9247236656865260862, -0.009046335405372961727, -0.3805316096397347025 ) ) ;
#7848 = ORIENTED_EDGE ( 'NONE', *, *, #426, .T. ) ;
#7849 = DIRECTION ( 'NONE',  ( 0.000000000000000000, 0.000000000000000000, -1.000000000000000000 ) ) ;
#7850 = CARTESIAN_POINT ( 'NONE',  ( -26.91620486903880050, 4.078357040894757368, 0.2218373908656702531 ) ) ;
#7851 = CARTESIAN_POINT ( 'NONE',  ( 37.00000000000000000, -3.673940397442057600E-15, -70.00000000000000000 ) ) ;
#7852 = DIRECTION ( 'NONE',  ( 0.000000000000000000, 0.000000000000000000, -1.000000000000000000 ) ) ;
#7853 = CIRCLE ( 'NONE', #782, 1.560000000000002274 ) ;
#7854 = CARTESIAN_POINT ( 'NONE',  ( 22.50000000000000355, 2.356749903719115078E-13, 5.000000000000000000 ) ) ;
#7855 = VERTEX_POINT ( 'NONE', #7964 ) ;
#7856 = EDGE_LOOP ( 'NONE', ( #8031, #2620 ) ) ;
#7857 = DIRECTION ( 'NONE',  ( -0.000000000000000000, -0.000000000000000000, -1.000000000000000000 ) ) ;
#7858 = ORIENTED_EDGE ( 'NONE', *, *, #4940, .F. ) ;
#7859 = EDGE_CURVE ( 'NONE', #1986, #1900, #2777, .T. ) ;
#7860 = CARTESIAN_POINT ( 'NONE',  ( 30.00000000000000000, 3.673940397442059178E-15, 10.00000000000000000 ) ) ;
#7861 = DIRECTION ( 'NONE',  ( -1.000000000000000000, 0.000000000000000000, 0.000000000000000000 ) ) ;
#7862 = CARTESIAN_POINT ( 'NONE',  ( 0.000000000000000000, 0.000000000000000000, 10.00000000000000000 ) ) ;
#7863 = DIRECTION ( 'NONE',  ( -1.000000000000000000, -0.000000000000000000, -0.000000000000000000 ) ) ;
#7864 = EDGE_CURVE ( 'NONE', #7578, #6441, #7091, .T. ) ;
#7865 = AXIS2_PLACEMENT_3D ( 'NONE', #1785, #1067, #257 ) ;
#7866 = LINE ( 'NONE', #611, #7114 ) ;
#7867 = FACE_OUTER_BOUND ( 'NONE', #2504, .T. ) ;
#7868 = ORIENTED_EDGE ( 'NONE', *, *, #7439, .F. ) ;
#7869 = ORIENTED_EDGE ( 'NONE', *, *, #1178, .T. ) ;
#7870 = FACE_OUTER_BOUND ( 'NONE', #9066, .T. ) ;
#7871 = ITEM_DEFINED_TRANSFORMATION ( 'NONE', 'NONE', #9441,  #1614 ) ;
#7872 = AXIS2_PLACEMENT_3D ( 'NONE', #5626, #3498, #2788 ) ;
#7873 = CARTESIAN_POINT ( 'NONE',  ( 0.000000000000000000, 22.50000000000000355, 10.00000000000000000 ) ) ;
#7874 = CARTESIAN_POINT ( 'NONE',  ( -22.50000000000000355, 0.000000000000000000, 10.00000000000000000 ) ) ;
#7875 = DIRECTION ( 'NONE',  ( -1.000000000000000000, 0.000000000000000000, 0.000000000000000000 ) ) ;
#7876 = CARTESIAN_POINT ( 'NONE',  ( 0.000000000000000000, -9.628187502531647418E-13, -19.99999999999950262 ) ) ;
#7877 = ORIENTED_EDGE ( 'NONE', *, *, #3127, .T. ) ;
#7878 = EDGE_LOOP ( 'NONE', ( #1244, #7664 ) ) ;
#7879 = ORIENTED_EDGE ( 'NONE', *, *, #8122, .F. ) ;
#7880 =( BOUNDED_CURVE ( )  B_SPLINE_CURVE ( 3, ( #3340, #2581, #5512, #405 ),
 .UNSPECIFIED., .F., .F. ) 
 B_SPLINE_CURVE_WITH_KNOTS ( ( 4, 4 ),
 ( 5.497787143782137953, 6.283185307179586232 ),
 .UNSPECIFIED. ) 
 CURVE ( )  GEOMETRIC_REPRESENTATION_ITEM ( )  RATIONAL_B_SPLINE_CURVE ( ( 1.000000000000000000, 0.9492530216741911220, 0.9492530216741911220, 1.000000000000000000 ) ) 
 REPRESENTATION_ITEM ( '' )  );
#7881 = VERTEX_POINT ( 'NONE', #7905 ) ;
#7882 = EDGE_CURVE ( 'NONE', #1471, #7477, #4388, .T. ) ;
#7883 = CARTESIAN_POINT ( 'NONE',  ( 0.000000000000000000, 0.000000000000000000, 11.99999999999999645 ) ) ;
#7884 = DIRECTION ( 'NONE',  ( 0.000000000000000000, -1.000000000000000000, 0.000000000000000000 ) ) ;
#7885 = PLANE ( 'NONE',  #610 ) ;
#7886 = FACE_OUTER_BOUND ( 'NONE', #6095, .T. ) ;
#7887 = CIRCLE ( 'NONE', #3746, 6.000000000000001776 ) ;
#7888 = CARTESIAN_POINT ( 'NONE',  ( 4.000000000000000000, 0.000000000000000000, 0.000000000000000000 ) ) ;
#7889 = ORIENTED_EDGE ( 'NONE', *, *, #5015, .F. ) ;
#7890 = DIRECTION ( 'NONE',  ( -1.000000000000000000, -0.000000000000000000, -0.000000000000000000 ) ) ;
#7891 = CIRCLE ( 'NONE', #3749, 22.50000000000000000 ) ;
#7892 = ORIENTED_EDGE ( 'NONE', *, *, #9124, .F. ) ;
#7893 = CARTESIAN_POINT ( 'NONE',  ( 0.000000000000000000, 0.000000000000000000, 8.000000000000005329 ) ) ;
#7894 = LINE ( 'NONE', #8572, #8385 ) ;
#7895 = DIRECTION ( 'NONE',  ( 1.000000000000000000, -0.000000000000000000, -0.000000000000000000 ) ) ;
#7896 = AXIS2_PLACEMENT_3D ( 'NONE', #2553, #3849, #6118 ) ;
#7897 = LINE ( 'NONE', #498, #9115 ) ;
#7898 = DIRECTION ( 'NONE',  ( 1.000000000000000000, 0.000000000000000000, 0.000000000000000000 ) ) ;
#7899 = VERTEX_POINT ( 'NONE', #8003 ) ;
#7900 = ORIENTED_EDGE ( 'NONE', *, *, #3897, .T. ) ;
#7901 = CARTESIAN_POINT ( 'NONE',  ( -0.4367635713301901701, 28.48785780768279707, 1.490418226835894755 ) ) ;
#7902 = ORIENTED_EDGE ( 'NONE', *, *, #5342, .F. ) ;
#7903 = DIRECTION ( 'NONE',  ( 0.7071067811865487940, 8.659560562354950115E-17, -0.7071067811865463515 ) ) ;
#7904 = CARTESIAN_POINT ( 'NONE',  ( 38.00000000000000000, 43.00000000000000000, 11.99999999999999645 ) ) ;
#7905 = CARTESIAN_POINT ( 'NONE',  ( -31.99999999999999289, 29.99999999999997868, 5.000000000000004441 ) ) ;
#7906 = CARTESIAN_POINT ( 'NONE',  ( 0.000000000000000000, 35.00000000000000000, 50.50000000000000000 ) ) ;
#7907 = AXIS2_PLACEMENT_3D ( 'NONE', #7710, #5551, #1116 ) ;
#7908 = EDGE_CURVE ( 'NONE', #5068, #2924, #7186, .T. ) ;
#7909 = CARTESIAN_POINT ( 'NONE',  ( -0.7500000000000000000, 0.7500000000000000000, 0.000000000000000000 ) ) ;
#7910 = LINE ( 'NONE', #5713, #3486 ) ;
#7911 = EDGE_CURVE ( 'NONE', #9473, #7366, #4206, .T. ) ;
#7912 = VERTEX_POINT ( 'NONE', #3436 ) ;
#7913 = ORIENTED_EDGE ( 'NONE', *, *, #613, .T. ) ;
#7914 = CIRCLE ( 'NONE', #7005, 3.000000000000002665 ) ;
#7915 = FACE_OUTER_BOUND ( 'NONE', #5209, .T. ) ;
#7916 = ADVANCED_FACE ( 'NONE', ( #5757 ), #2865, .F. ) ;
#7917 = PRODUCT_DEFINITION_SHAPE ( 'NONE', 'NONE',  #9483 ) ;
#7918 = CARTESIAN_POINT ( 'NONE',  ( -22.50000000000000000, -7.855833012397050680E-14, 0.000000000000000000 ) ) ;
#7919 = AXIS2_PLACEMENT_3D ( 'NONE', #3727, #1514, #4595 ) ;
#7920 = LINE ( 'NONE', #2747, #2359 ) ;
#7921 = FACE_OUTER_BOUND ( 'NONE', #1702, .T. ) ;
#7922 = VERTEX_POINT ( 'NONE', #3533 ) ;
#7923 = EDGE_LOOP ( 'NONE', ( #5364, #2861, #164, #8073 ) ) ;
#7924 = EDGE_CURVE ( 'NONE', #3451, #6084, #4702, .T. ) ;
#7925 = ORIENTED_EDGE ( 'NONE', *, *, #3548, .T. ) ;
#7926 = ORIENTED_EDGE ( 'NONE', *, *, #4842, .T. ) ;
#7927 = CIRCLE ( 'NONE', #6406, 1.559999999998939346 ) ;
#7928 = CARTESIAN_POINT ( 'NONE',  ( 28.32042821893189455, -1.471975546721147721, 1.357900206176151370 ) ) ;
#7929 = CARTESIAN_POINT ( 'NONE',  ( 18.50000000000001776, 2.265596578422605368E-15, 0.000000000000000000 ) ) ;
#7930 = VECTOR ( 'NONE', #7936, 1000.000000000000114 ) ;
#7931 = LINE ( 'NONE', #1932, #5193 ) ;
#7932 = CARTESIAN_POINT ( 'NONE',  ( -28.75000000000002132, 2.329604860730800488E-26, 1.750000000000023537 ) ) ;
#7933 = EDGE_CURVE ( 'NONE', #672, #3936, #5922, .T. ) ;
#7934 = VECTOR ( 'NONE', #3700, 1000.000000000000000 ) ;
#7935 = ADVANCED_FACE ( 'NONE', ( #6383 ), #1269, .F. ) ;
#7936 = DIRECTION ( 'NONE',  ( -0.7071067811865461294, 0.7071067811865489050, -3.960316634274389414E-15 ) ) ;
#7937 =( BOUNDED_CURVE ( )  B_SPLINE_CURVE ( 3, ( #4465, #7389, #4420, #5085 ),
 .UNSPECIFIED., .F., .F. ) 
 B_SPLINE_CURVE_WITH_KNOTS ( ( 4, 4 ),
 ( 5.831078311124174185, 6.735292303234999167 ),
 .UNSPECIFIED. ) 
 CURVE ( )  GEOMETRIC_REPRESENTATION_ITEM ( )  RATIONAL_B_SPLINE_CURVE ( ( 1.000000000000000000, 0.9330190890865965869, 0.9330190890865965869, 1.000000000000000000 ) ) 
 REPRESENTATION_ITEM ( '' )  );
#7938 = VECTOR ( 'NONE', #7627, 999.9999999999998863 ) ;
#7939 = ORIENTED_EDGE ( 'NONE', *, *, #5243, .T. ) ;
#7940 = EDGE_CURVE ( 'NONE', #580, #900, #5708, .T. ) ;
#7941 = FACE_OUTER_BOUND ( 'NONE', #2041, .T. ) ;
#7942 = EDGE_CURVE ( 'NONE', #7512, #3144, #6519, .T. ) ;
#7943 = EDGE_CURVE ( 'NONE', #1986, #4149, #3941, .T. ) ;
#7944 = ORIENTED_EDGE ( 'NONE', *, *, #3711, .T. ) ;
#7945 = AXIS2_PLACEMENT_3D ( 'NONE', #1568, #5803, #8732 ) ;
#7946 = CARTESIAN_POINT ( 'NONE',  ( 19.50000000000000355, 0.000000000000000000, 10.00000000000000000 ) ) ;
#7947 = CARTESIAN_POINT ( 'NONE',  ( -28.50000000000000000, 0.4241759143235341312, 1.500000000000036859 ) ) ;
#7948 = TOROIDAL_SURFACE ( 'NONE', #3801, 5.000000000000000888, 1.000000000000000000 ) ;
#7949 = CARTESIAN_POINT ( 'NONE',  ( -6.000000000000000888, 22.50000000000000355, 2.000000000000013767 ) ) ;
#7950 = AXIS2_PLACEMENT_3D ( 'NONE', #5329, #7480, #8061 ) ;
#7951 = CARTESIAN_POINT ( 'NONE',  ( 25.50000000000000355, 2.360423844116556880E-13, 10.00000000000000000 ) ) ;
#7952 = CARTESIAN_POINT ( 'NONE',  ( -3.157268078127657862, -27.61694991999679871, 0.7947205175373147634 ) ) ;
#7953 = ORIENTED_EDGE ( 'NONE', *, *, #8210, .F. ) ;
#7954 = EDGE_CURVE ( 'NONE', #6860, #9262, #8538, .T. ) ;
#7955 = ORIENTED_EDGE ( 'NONE', *, *, #4124, .F. ) ;
#7956 = CARTESIAN_POINT ( 'NONE',  ( 37.00000000000000000, -21.98223304703365244, -86.98223304703364533 ) ) ;
#7957 = ORIENTED_EDGE ( 'NONE', *, *, #1008, .F. ) ;
#7958 = EDGE_CURVE ( 'NONE', #8859, #490, #5891, .T. ) ;
#7959 = DIRECTION ( 'NONE',  ( -1.000000000000000000, 0.000000000000000000, 0.000000000000000000 ) ) ;
#7960 = CARTESIAN_POINT ( 'NONE',  ( -5.000000000000000888, 6.123233995736767268E-16, 4.000000000000000000 ) ) ;
#7961 = CIRCLE ( 'NONE', #3495, 1.560000000002327303 ) ;
#7962 = CIRCLE ( 'NONE', #5808, 7.250000000000002665 ) ;
#7963 = EDGE_CURVE ( 'NONE', #490, #3514, #951, .T. ) ;
#7964 = CARTESIAN_POINT ( 'NONE',  ( 0.000000000000000000, -18.47759065022790637, -8.403668647301127947 ) ) ;
#7965 = AXIS2_PLACEMENT_3D ( 'NONE', #5094, #7255, #5245 ) ;
#7966 = FACE_BOUND ( 'NONE', #3675, .T. ) ;
#7967 = DIRECTION ( 'NONE',  ( 0.000000000000000000, 0.000000000000000000, 1.000000000000000000 ) ) ;
#7968 = DIRECTION ( 'NONE',  ( -1.000000000000000000, 0.000000000000000000, 0.000000000000000000 ) ) ;
#7969 = ORIENTED_EDGE ( 'NONE', *, *, #1413, .F. ) ;
#7970 = VERTEX_POINT ( 'NONE', #38 ) ;
#7971 = DIRECTION ( 'NONE',  ( 0.000000000000000000, 0.000000000000000000, -1.000000000000000000 ) ) ;
#7972 = ITEM_DEFINED_TRANSFORMATION ( 'NONE', 'NONE', #7760,  #1614 ) ;
#7973 = CARTESIAN_POINT ( 'NONE',  ( 11.96410161513786008, 1.497994186849708771E-15, 50.00000000000000000 ) ) ;
#7974 = CARTESIAN_POINT ( 'NONE',  ( 0.000000000000000000, -22.50000000000000355, 2.000000000000013767 ) ) ;
#7975 = DIRECTION ( 'NONE',  ( -1.000000000000000000, -0.000000000000000000, -0.000000000000000000 ) ) ;
#7976 = VERTEX_POINT ( 'NONE', #4451 ) ;
#7977 = ORIENTED_EDGE ( 'NONE', *, *, #3257, .F. ) ;
#7978 = ORIENTED_EDGE ( 'NONE', *, *, #8930, .T. ) ;
#7979 = ORIENTED_EDGE ( 'NONE', *, *, #251, .T. ) ;
#7980 = CARTESIAN_POINT ( 'NONE',  ( -2.818925648462311528E-15, -3.500000000000000000, 0.000000000000000000 ) ) ;
#7981 = PLANE ( 'NONE',  #3480 ) ;
#7982 = DIRECTION ( 'NONE',  ( 0.7071067811865505703, 0.7071067811865444641, -0.000000000000000000 ) ) ;
#7983 = FACE_OUTER_BOUND ( 'NONE', #6674, .T. ) ;
#7984 = FACE_OUTER_BOUND ( 'NONE', #4250, .T. ) ;
#7985 = VECTOR ( 'NONE', #5892, 1000.000000000000114 ) ;
#7986 = ORIENTED_EDGE ( 'NONE', *, *, #6576, .F. ) ;
#7987 = DIRECTION ( 'NONE',  ( 0.000000000000000000, 0.000000000000000000, 1.000000000000000000 ) ) ;
#7988 = ORIENTED_EDGE ( 'NONE', *, *, #15, .F. ) ;
#7989 = DIRECTION ( 'NONE',  ( -1.000000000000000000, 0.000000000000000000, 0.000000000000000000 ) ) ;
#7990 = CARTESIAN_POINT ( 'NONE',  ( 5.000000000000000000, 20.00000000000120437, 7.412591687719288072E-13 ) ) ;
#7991 = CIRCLE ( 'NONE', #627, 22.50000000000000000 ) ;
#7992 = CARTESIAN_POINT ( 'NONE',  ( -2.749999999999995559, 0.7500000000000000000, 0.000000000000000000 ) ) ;
#7993 = EDGE_CURVE ( 'NONE', #5804, #5660, #8241, .T. ) ;
#7994 = CARTESIAN_POINT ( 'NONE',  ( 37.00000000000000000, -1.836970198721028011E-15, -85.00000000000000000 ) ) ;
#7995 = EDGE_CURVE ( 'NONE', #8566, #1694, #6662, .T. ) ;
#7996 = CARTESIAN_POINT ( 'NONE',  ( 3.795548148769905428, -27.16282829747748195, 0.4246316111951826677 ) ) ;
#7997 = ORIENTED_EDGE ( 'NONE', *, *, #2810, .T. ) ;
#7998 = VERTEX_POINT ( 'NONE', #4492 ) ;
#7999 = CARTESIAN_POINT ( 'NONE',  ( -37.00000000000000711, -15.90990257669733943, -82.90990257669729147 ) ) ;
#8000 = ORIENTED_EDGE ( 'NONE', *, *, #7530, .T. ) ;
#8001 = CARTESIAN_POINT ( 'NONE',  ( 30.00000000000000000, 0.000000000000000000, 2.999999999999999112 ) ) ;
#8002 = LINE ( 'NONE', #1414, #139 ) ;
#8003 = CARTESIAN_POINT ( 'NONE',  ( 0.000000000000000000, -17.50000000000000000, 49.50000000000000000 ) ) ;
#8004 = CIRCLE ( 'NONE', #5404, 8.000000000000047962 ) ;
#8005 = CARTESIAN_POINT ( 'NONE',  ( 37.00000000000000000, 15.90990257669733943, -51.09009742330271564 ) ) ;
#8006 = EDGE_CURVE ( 'NONE', #8784, #2406, #178, .T. ) ;
#8007 = CARTESIAN_POINT ( 'NONE',  ( -19.62310601229373574, -19.62310601229373574, 26.87436867076458924 ) ) ;
#8008 = DIRECTION ( 'NONE',  ( -1.000000000000000000, 0.000000000000000000, 0.000000000000000000 ) ) ;
#8009 = ORIENTED_EDGE ( 'NONE', *, *, #7940, .T. ) ;
#8010 = ORIENTED_EDGE ( 'NONE', *, *, #2901, .F. ) ;
#8011 = PRESENTATION_LAYER_ASSIGNMENT (  '', '', ( #2341 ) ) ;
#8012 = PLANE ( 'NONE',  #417 ) ;
#8013 = VECTOR ( 'NONE', #9369, 1000.000000000000000 ) ;
#8014 = CARTESIAN_POINT ( 'NONE',  ( 3.500000000000000444, -6.505213034913026604E-16, 1.500000000000000000 ) ) ;
#8015 = CARTESIAN_POINT ( 'NONE',  ( 38.00000000000000000, -43.00000000000000000, -7.366666666666667140 ) ) ;
#8016 = CARTESIAN_POINT ( 'NONE',  ( -60.00000000000000000, 0.000000000000000000, -30.00000000000000000 ) ) ;
#8017 = ORIENTED_EDGE ( 'NONE', *, *, #9339, .T. ) ;
#8018 = ORIENTED_EDGE ( 'NONE', *, *, #5890, .T. ) ;
#8019 = VECTOR ( 'NONE', #1662, 1000.000000000000000 ) ;
#8020 = ORIENTED_EDGE ( 'NONE', *, *, #3608, .T. ) ;
#8021 = DIRECTION ( 'NONE',  ( -1.000000000000000000, 0.000000000000000000, 0.000000000000000000 ) ) ;
#8022 = ORIENTED_EDGE ( 'NONE', *, *, #8055, .F. ) ;
#8023 = CARTESIAN_POINT ( 'NONE',  ( 27.61492299646195647, -3.160432959937327535, 0.7930775300198846800 ) ) ;
#8024 = DIRECTION ( 'NONE',  ( 0.000000000000000000, 0.000000000000000000, 1.000000000000000000 ) ) ;
#8025 = CARTESIAN_POINT ( 'NONE',  ( 22.50000000000000355, 0.000000000000000000, 5.000000000000000000 ) ) ;
#8026 = AXIS2_PLACEMENT_3D ( 'NONE', #6512, #7268, #2904 ) ;
#8027 = CARTESIAN_POINT ( 'NONE',  ( 0.000000000000000000, 20.00000000000120437, -1.559999999998198161 ) ) ;
#8028 = LINE ( 'NONE', #5971, #5370 ) ;
#8029 = ADVANCED_FACE ( 'NONE', ( #3000, #5845 ), #3100, .T. ) ;
#8030 = DIRECTION ( 'NONE',  ( -0.000000000000000000, -0.000000000000000000, -1.000000000000000000 ) ) ;
#8031 = ORIENTED_EDGE ( 'NONE', *, *, #2347, .T. ) ;
#8032 = DIRECTION ( 'NONE',  ( 0.000000000000000000, -0.7071067811865479058, 0.7071067811865472397 ) ) ;
#8033 = ORIENTED_EDGE ( 'NONE', *, *, #331, .F. ) ;
#8034 = DIRECTION ( 'NONE',  ( -0.000000000000000000, -0.000000000000000000, -1.000000000000000000 ) ) ;
#8035 = EDGE_CURVE ( 'NONE', #4149, #1986, #8230, .T. ) ;
#8036 = LINE ( 'NONE', #737, #8242 ) ;
#8037 = DIRECTION ( 'NONE',  ( 0.000000000000000000, 0.9175556253099241832, -0.3976074376343005090 ) ) ;
#8038 = CARTESIAN_POINT ( 'NONE',  ( 4.000000000000000000, 7.653668647302530381, 17.72759065022973246 ) ) ;
#8039 = AXIS2_PLACEMENT_3D ( 'NONE', #3382, #1170, #7043 ) ;
#8040 = EDGE_LOOP ( 'NONE', ( #7310, #6657, #4991, #7449, #3250 ) ) ;
#8041 = VERTEX_POINT ( 'NONE', #6571 ) ;
#8042 =( LENGTH_UNIT ( ) NAMED_UNIT ( * ) SI_UNIT ( .MILLI., .METRE. ) );
#8043 = ORIENTED_EDGE ( 'NONE', *, *, #7943, .T. ) ;
#8044 = DIRECTION ( 'NONE',  ( 0.000000000000000000, 0.000000000000000000, 1.000000000000000000 ) ) ;
#8045 = AXIS2_PLACEMENT_3D ( 'NONE', #3062, #133, #7967 ) ;
#8046 = CARTESIAN_POINT ( 'NONE',  ( 60.00000000000000000, -3.673940397442057600E-15, -55.00000000000000711 ) ) ;
#8047 = CARTESIAN_POINT ( 'NONE',  ( 60.00000000000001421, 9.637301612213116542, -29.99999999999998934 ) ) ;
#8048 = AXIS2_PLACEMENT_3D ( 'NONE', #2913, #9211, #4851 ) ;
#8049 = CARTESIAN_POINT ( 'NONE',  ( 0.000000000000000000, 18.47759065022580316, -7.653668647301631545 ) ) ;
#8050 = FACE_OUTER_BOUND ( 'NONE', #2202, .T. ) ;
#8051 = PRODUCT_DEFINITION ( 'UNKNOWN', '', #1002, #6732 ) ;
#8052 = EDGE_CURVE ( 'NONE', #6279, #8200, #7467, .T. ) ;
#8053 = DIRECTION ( 'NONE',  ( -1.000000000000000000, 0.000000000000000000, 0.000000000000000000 ) ) ;
#8054 = CARTESIAN_POINT ( 'NONE',  ( 5.000000000000000000, 14.14213562373112154, -12.58213562373077821 ) ) ;
#8055 = EDGE_CURVE ( 'NONE', #287, #8464, #7009, .T. ) ;
#8056 = EDGE_LOOP ( 'NONE', ( #6050, #2253, #172, #2840 ) ) ;
#8057 = ADVANCED_FACE ( 'NONE', ( #8812 ), #129, .F. ) ;
#8058 = EDGE_LOOP ( 'NONE', ( #987, #1356, #743, #735 ) ) ;
#8059 = CARTESIAN_POINT ( 'NONE',  ( 6.000000000000000888, -22.50000000000000355, 2.000000000000013767 ) ) ;
#8060 = ADVANCED_BREP_SHAPE_REPRESENTATION ( '', ( #4990, #1614 ), #1322 ) ;
#8061 = DIRECTION ( 'NONE',  ( 1.000000000000000000, 0.000000000000000000, 0.000000000000000000 ) ) ;
#8062 = EDGE_CURVE ( 'NONE', #2916, #4498, #3780, .T. ) ;
#8063 = PRODUCT_DEFINITION_FORMATION_WITH_SPECIFIED_SOURCE ( 'ANY', '', #7384, .NOT_KNOWN. ) ;
#8064 = DIRECTION ( 'NONE',  ( 0.000000000000000000, 0.000000000000000000, -1.000000000000000000 ) ) ;
#8065 = ADVANCED_FACE ( 'NONE', ( #8770 ), #2400, .T. ) ;
#8066 = FACE_OUTER_BOUND ( 'NONE', #7023, .T. ) ;
#8067 = PRODUCT_DEFINITION_FORMATION_WITH_SPECIFIED_SOURCE ( 'ANY', '', #4471, .NOT_KNOWN. ) ;
#8068 = ORIENTED_EDGE ( 'NONE', *, *, #5673, .F. ) ;
#8069 = VERTEX_POINT ( 'NONE', #5115 ) ;
#8070 = VERTEX_POINT ( 'NONE', #4543 ) ;
#8071 = EDGE_CURVE ( 'NONE', #3554, #2947, #747, .T. ) ;
#8072 = CARTESIAN_POINT ( 'NONE',  ( -56.07586385285966202, 96.36314398677647830, 28.04625972167943004 ) ) ;
#8073 = ORIENTED_EDGE ( 'NONE', *, *, #8651, .F. ) ;
#8074 = DIRECTION ( 'NONE',  ( -0.000000000000000000, -0.000000000000000000, -1.000000000000000000 ) ) ;
#8075 = CARTESIAN_POINT ( 'NONE',  ( 52.86930915046634283, 28.38475884032109775, -81.18159060786257442 ) ) ;
#8076 = CIRCLE ( 'NONE', #4852, 3.000000000000000000 ) ;
#8077 = DIRECTION ( 'NONE',  ( 0.000000000000000000, 0.000000000000000000, -1.000000000000000000 ) ) ;
#8078 = PRODUCT_DEFINITION_SHAPE ( 'NONE', 'NONE',  #9495 ) ;
#8079 = DIRECTION ( 'NONE',  ( 0.000000000000000000, 0.000000000000000000, -1.000000000000000000 ) ) ;
#8080 = DIRECTION ( 'NONE',  ( 0.000000000000000000, 0.000000000000000000, -1.000000000000000000 ) ) ;
#8081 = LINE ( 'NONE', #3707, #2099 ) ;
#8082 = VERTEX_POINT ( 'NONE', #8958 ) ;
#8083 = AXIS2_PLACEMENT_3D ( 'NONE', #8908, #3058, #5270 ) ;
#8084 = DIRECTION ( 'NONE',  ( -0.000000000000000000, -0.000000000000000000, -1.000000000000000000 ) ) ;
#8085 = ORIENTED_EDGE ( 'NONE', *, *, #1072, .T. ) ;
#8086 = DIRECTION ( 'NONE',  ( 1.000000000000000000, 0.000000000000000000, 0.000000000000000000 ) ) ;
#8087 = CARTESIAN_POINT ( 'NONE',  ( 22.50000000000000355, 0.000000000000000000, 2.000000000000035083 ) ) ;
#8088 = VECTOR ( 'NONE', #4989, 1000.000000000000000 ) ;
#8089=STYLED_ITEM('',(#9515),#171);
#8090 = CARTESIAN_POINT ( 'NONE',  ( -5.999999999999842792, -22.50000000000000355, 5.000000000000000000 ) ) ;
#8091 = CIRCLE ( 'NONE', #9303, 16.00000000000000000 ) ;
#8092 = CARTESIAN_POINT ( 'NONE',  ( 0.000000000000000000, 2.724839128102860991E-15, 22.00000000000000711 ) ) ;
#8093 = VECTOR ( 'NONE', #1, 1000.000000000000114 ) ;
#8094 = ORIENTED_EDGE ( 'NONE', *, *, #1049, .F. ) ;
#8095 = VECTOR ( 'NONE', #4979, 1000.000000000000000 ) ;
#8096 = ORIENTED_EDGE ( 'NONE', *, *, #4139, .F. ) ;
#8097 = CARTESIAN_POINT ( 'NONE',  ( 4.077745023575991112, 26.91684391854055036, 0.2223699321171545285 ) ) ;
#8098 = CIRCLE ( 'NONE', #3960, 3.000000000000002665 ) ;
#8099 = EDGE_LOOP ( 'NONE', ( #9195, #4016, #7812 ) ) ;
#8100 = VECTOR ( 'NONE', #1488, 1000.000000000000000 ) ;
#8101 = CARTESIAN_POINT ( 'NONE',  ( -53.29490495164537833, 27.56180520566615044, -134.0000000000000284 ) ) ;
#8102 = LINE ( 'NONE', #5164, #4427 ) ;
#8103 = LINE ( 'NONE', #7519, #9141 ) ;
#8104 = VECTOR ( 'NONE', #3928, 1000.000000000000114 ) ;
#8105 = DIRECTION ( 'NONE',  ( 1.000000000000000000, 0.000000000000000000, 0.000000000000000000 ) ) ;
#8106 = FACE_OUTER_BOUND ( 'NONE', #4589, .T. ) ;
#8107 = DIRECTION ( 'NONE',  ( -1.000000000000000000, 0.000000000000000000, 0.000000000000000000 ) ) ;
#8108 = DIRECTION ( 'NONE',  ( 0.000000000000000000, 0.000000000000000000, -1.000000000000000000 ) ) ;
#8109 = ORIENTED_EDGE ( 'NONE', *, *, #8640, .T. ) ;
#8110 = ORIENTED_EDGE ( 'NONE', *, *, #8618, .T. ) ;
#8111 = AXIS2_PLACEMENT_3D ( 'NONE', #8149, #1563, #3056 ) ;
#8112 = CARTESIAN_POINT ( 'NONE',  ( 0.000000000000000000, 0.000000000000000000, 5.000000000000000000 ) ) ;
#8113 = CARTESIAN_POINT ( 'NONE',  ( -6.000000000000000888, 22.50000000000000355, 2.000000000000013767 ) ) ;
#8114 = ORIENTED_EDGE ( 'NONE', *, *, #4139, .T. ) ;
#8115 = CARTESIAN_POINT ( 'NONE',  ( -6.697288230627575167, 26.42764960499151528, 0.2570604603516986608 ) ) ;
#8116 = EDGE_CURVE ( 'NONE', #7524, #6045, #5928, .T. ) ;
#8117 = CIRCLE ( 'NONE', #9028, 0.7499999999982936982 ) ;
#8118 = EDGE_CURVE ( 'NONE', #4695, #3685, #5634, .T. ) ;
#8119 = VECTOR ( 'NONE', #4443, 1000.000000000000000 ) ;
#8120 = FACE_BOUND ( 'NONE', #2749, .T. ) ;
#8121 = EDGE_CURVE ( 'NONE', #550, #5932, #8103, .T. ) ;
#8122 = EDGE_CURVE ( 'NONE', #8200, #523, #7714, .T. ) ;
#8123 = CARTESIAN_POINT ( 'NONE',  ( 4.000000000000000000, -20.00000000000120437, 2.661998082081668380E-12 ) ) ;
#8124 = ORIENTED_EDGE ( 'NONE', *, *, #4830, .T. ) ;
#8125 = EDGE_LOOP ( 'NONE', ( #1087, #5584, #6450, #5136 ) ) ;
#8126 =( NAMED_UNIT ( * ) SI_UNIT ( $, .STERADIAN. ) SOLID_ANGLE_UNIT ( ) );
#8127 = VERTEX_POINT ( 'NONE', #2486 ) ;
#8128 = FACE_OUTER_BOUND ( 'NONE', #5613, .T. ) ;
#8129 = DIRECTION ( 'NONE',  ( 1.000000000000000000, -0.000000000000000000, -0.000000000000000000 ) ) ;
#8130 = DIRECTION ( 'NONE',  ( 0.000000000000000000, 0.000000000000000000, -1.000000000000000000 ) ) ;
#8131 = CARTESIAN_POINT ( 'NONE',  ( 3.000000000000156763, -22.50000000000000355, 10.00000000000000000 ) ) ;
#8132 = DIRECTION ( 'NONE',  ( 1.000000000000000000, -0.000000000000000000, -0.000000000000000000 ) ) ;
#8133 = CARTESIAN_POINT ( 'NONE',  ( -2.750000000000002665, -0.7500000000000000000, 1.500000000000000000 ) ) ;
#8134 = ADVANCED_FACE ( 'NONE', ( #8482 ), #1851, .F. ) ;
#8135 = EDGE_LOOP ( 'NONE', ( #8554, #1927, #8607, #3827 ) ) ;
#8136 = DIRECTION ( 'NONE',  ( 1.000000000000000000, 0.000000000000000000, 0.000000000000000000 ) ) ;
#8137 = ORIENTED_EDGE ( 'NONE', *, *, #4261, .F. ) ;
#8138 = FACE_BOUND ( 'NONE', #4685, .T. ) ;
#8139 = PLANE ( 'NONE',  #1177 ) ;
#8140 = EDGE_CURVE ( 'NONE', #3779, #9178, #6142, .T. ) ;
#8141 = DIRECTION ( 'NONE',  ( 0.000000000000000000, -1.000000000000000000, 0.000000000000000000 ) ) ;
#8142 = CARTESIAN_POINT ( 'NONE',  ( -17.49999999999999645, 4.703319286132084720, 49.50000000000000000 ) ) ;
#8143 = VERTEX_POINT ( 'NONE', #223 ) ;
#8144 = ORIENTED_EDGE ( 'NONE', *, *, #3656, .T. ) ;
#8145 = ORIENTED_EDGE ( 'NONE', *, *, #7110, .T. ) ;
#8146 =( NAMED_UNIT ( * ) SI_UNIT ( $, .STERADIAN. ) SOLID_ANGLE_UNIT ( ) );
#8147 = VERTEX_POINT ( 'NONE', #5458 ) ;
#8148 = LINE ( 'NONE', #8101, #2286 ) ;
#8149 = CARTESIAN_POINT ( 'NONE',  ( 1.571166602479410136E-13, -22.50000000000000355, 5.000000000000000000 ) ) ;
#8150 = VECTOR ( 'NONE', #2500, 1000.000000000000114 ) ;
#8151 = CARTESIAN_POINT ( 'NONE',  ( 53.29490495164537833, 27.56180520566613268, -41.61356529332876875 ) ) ;
#8152 = DIRECTION ( 'NONE',  ( 0.000000000000000000, 0.000000000000000000, -1.000000000000000000 ) ) ;
#8153 = LINE ( 'NONE', #1567, #2378 ) ;
#8154 = DIRECTION ( 'NONE',  ( -0.000000000000000000, -0.000000000000000000, -1.000000000000000000 ) ) ;
#8155 = ADVANCED_FACE ( 'NONE', ( #5410 ), #6088, .T. ) ;
#8156 = ORIENTED_EDGE ( 'NONE', *, *, #8614, .F. ) ;
#8157 = ORIENTED_EDGE ( 'NONE', *, *, #7942, .F. ) ;
#8158 = DIRECTION ( 'NONE',  ( -0.000000000000000000, -0.000000000000000000, 1.000000000000000000 ) ) ;
#8159 = ORIENTED_EDGE ( 'NONE', *, *, #1178, .F. ) ;
#8160 = VECTOR ( 'NONE', #7364, 1000.000000000000000 ) ;
#8161 = PRODUCT_DEFINITION_SHAPE ( 'NONE', 'NONE',  #7762 ) ;
#8162 = EDGE_CURVE ( 'NONE', #8254, #9088, #9450, .T. ) ;
#8163 = CARTESIAN_POINT ( 'NONE',  ( 4.208878922505766340, 27.87018698802495464, 1.184405920873192075 ) ) ;
#8164 = FACE_OUTER_BOUND ( 'NONE', #2357, .T. ) ;
#8165 = CARTESIAN_POINT ( 'NONE',  ( -15.00000000000000000, 0.000000000000000000, 11.00000000000000000 ) ) ;
#8166 = VERTEX_POINT ( 'NONE', #8383 ) ;
#8167 = ORIENTED_EDGE ( 'NONE', *, *, #8322, .T. ) ;
#8168 = CARTESIAN_POINT ( 'NONE',  ( 22.66898259762508872, 143.3415266320050989, 26.09957017205283591 ) ) ;
#8169 = CARTESIAN_POINT ( 'NONE',  ( -53.29490495164537833, 15.90990257669733943, -82.90990257669729147 ) ) ;
#8170 = DIRECTION ( 'NONE',  ( 1.000000000000000000, 0.000000000000000000, 0.000000000000000000 ) ) ;
#8171 = DIRECTION ( 'NONE',  ( -1.000000000000000000, 0.000000000000000000, 0.000000000000000000 ) ) ;
#8172 = DIRECTION ( 'NONE',  ( -0.7071067811865512365, 0.000000000000000000, -0.7071067811865439090 ) ) ;
#8173 = PLANE ( 'NONE',  #8731 ) ;
#8174 = DIRECTION ( 'NONE',  ( -1.000000000000000000, 0.000000000000000000, 0.000000000000000000 ) ) ;
#8175 = ADVANCED_FACE ( 'NONE', ( #938 ), #4018, .T. ) ;
#8176 = CARTESIAN_POINT ( 'NONE',  ( -2.254970896015736415, -28.06387613437635409, 1.153664892585073432 ) ) ;
#8177 = EDGE_CURVE ( 'NONE', #5087, #9340, #9296, .T. ) ;
#8178 = ORIENTED_EDGE ( 'NONE', *, *, #1123, .T. ) ;
#8179 = ORIENTED_EDGE ( 'NONE', *, *, #7667, .T. ) ;
#8180 = B_SPLINE_CURVE_WITH_KNOTS ( 'NONE', 3,
 ( #504, #6379, #5659, #8580, #4925, #9341, #5704, #8622, #4970, #7901, #8903, #8860, #4349, #3721, #5161, #3053, #7271, #4447, #6612, #32, #8097, #693 ),
 .UNSPECIFIED., .F., .F.,
 ( 4, 2, 2, 2, 2, 2, 2, 2, 2, 2, 4 ),
 ( 0.000000000000000000, 0.001276335940410827955, 0.002552671880821655911, 0.003829007821232484950, 0.004467175791437899036, 0.005105343761643314424, 0.006381679702054142596, 0.007019847672259558850, 0.007658015642464973370, 0.008934351582875805012, 0.01021068752328663752 ),
 .UNSPECIFIED. ) ;
#8181 = CARTESIAN_POINT ( 'NONE',  ( 38.00000000000000000, -43.00000000000000000, -7.366666666666667140 ) ) ;
#8182 = CARTESIAN_POINT ( 'NONE',  ( 4.119968255444916849E-15, 3.500000000000000000, 1.500000000000000000 ) ) ;
#8183 = AXIS2_PLACEMENT_3D ( 'NONE', #9125, #3366, #1691 ) ;
#8184 = LINE ( 'NONE', #1600, #3985 ) ;
#8185 = CARTESIAN_POINT ( 'NONE',  ( -17.50000000000000355, 2.143131898507868643E-15, 49.50000000000000000 ) ) ;
#8186 = VERTEX_POINT ( 'NONE', #4739 ) ;
#8187 = VERTEX_POINT ( 'NONE', #4783 ) ;
#8188 = AXIS2_PLACEMENT_3D ( 'NONE', #8442, #4199, #4112 ) ;
#8189 = VERTEX_POINT ( 'NONE', #1120 ) ;
#8190 = ORIENTED_EDGE ( 'NONE', *, *, #9419, .T. ) ;
#8191 = CARTESIAN_POINT ( 'NONE',  ( 4.000000000000000000, -18.47759065022790637, -8.403668647301127947 ) ) ;
#8192 = DIRECTION ( 'NONE',  ( 1.000000000000000000, 0.000000000000000000, 0.000000000000000000 ) ) ;
#8193 =( BOUNDED_CURVE ( )  B_SPLINE_CURVE ( 3, ( #1816, #7773, #6869, #3932 ),
 .UNSPECIFIED., .F., .F. ) 
 B_SPLINE_CURVE_WITH_KNOTS ( ( 4, 4 ),
 ( 5.831078311124173297, 6.735292303234999167 ),
 .UNSPECIFIED. ) 
 CURVE ( )  GEOMETRIC_REPRESENTATION_ITEM ( )  RATIONAL_B_SPLINE_CURVE ( ( 1.000000000000000000, 0.9330190890865963649, 0.9330190890865963649, 1.000000000000000000 ) ) 
 REPRESENTATION_ITEM ( '' )  );
#8194 = DIRECTION ( 'NONE',  ( 0.000000000000000000, 0.000000000000000000, -1.000000000000000000 ) ) ;
#8195 = VECTOR ( 'NONE', #2458, 1000.000000000000000 ) ;
#8196 = CARTESIAN_POINT ( 'NONE',  ( 0.000000000000000000, 0.000000000000000000, 5.000000000000000000 ) ) ;
#8197 = CARTESIAN_POINT ( 'NONE',  ( 12.37436867076458036, 12.37436867076458036, 19.62563132923542142 ) ) ;
#8198 = FILL_AREA_STYLE ('',( #7522 ) ) ;
#8199 = CARTESIAN_POINT ( 'NONE',  ( 37.22467645238198486, 47.05659850664387989, 11.99999999999999645 ) ) ;
#8200 = VERTEX_POINT ( 'NONE', #7668 ) ;
#8201 = AXIS2_PLACEMENT_3D ( 'NONE', #8263, #3989, #7538 ) ;
#8202 = EDGE_LOOP ( 'NONE', ( #1950, #6721 ) ) ;
#8203 = CARTESIAN_POINT ( 'NONE',  ( 4.333301281932778082, 26.64999999999997371, 0.000000000000000000 ) ) ;
#8204 = AXIS2_PLACEMENT_3D ( 'NONE', #7874, #1281, #4219 ) ;
#8205 = ORIENTED_EDGE ( 'NONE', *, *, #6833, .F. ) ;
#8206 = DIRECTION ( 'NONE',  ( -0.7071067811865455743, -1.057629477510965448E-15, 0.7071067811865493491 ) ) ;
#8207 = CARTESIAN_POINT ( 'NONE',  ( -37.00000000000000000, -30.00000000000000000, -78.96446609406729067 ) ) ;
#8208 = CARTESIAN_POINT ( 'NONE',  ( 2.663458823497500294, -28.40635703822599822, 1.529086667430999524 ) ) ;
#8209 = ORIENTED_EDGE ( 'NONE', *, *, #613, .F. ) ;
#8210 = EDGE_CURVE ( 'NONE', #6148, #4790, #6249, .T. ) ;
#8211 = ORIENTED_EDGE ( 'NONE', *, *, #8563, .F. ) ;
#8212 = AXIS2_PLACEMENT_3D ( 'NONE', #4392, #4075, #2949 ) ;
#8213 = DIRECTION ( 'NONE',  ( 1.000000000000000000, -1.222980050563648509E-16, -3.469446951953614189E-18 ) ) ;
#8214 = CARTESIAN_POINT ( 'NONE',  ( 0.000000000000000000, -20.00000000000120437, 2.661998082081668380E-12 ) ) ;
#8215 = DIRECTION ( 'NONE',  ( -0.000000000000000000, -0.000000000000000000, -1.000000000000000000 ) ) ;
#8216 = DIRECTION ( 'NONE',  ( -1.000000000000000000, -0.000000000000000000, -0.000000000000000000 ) ) ;
#8217 = LINE ( 'NONE', #5095, #645 ) ;
#8218 = ADVANCED_FACE ( 'NONE', ( #2440 ), #6098, .F. ) ;
#8219 = DIRECTION ( 'NONE',  ( -1.000000000000000000, -0.000000000000000000, -0.000000000000000000 ) ) ;
#8220 = CARTESIAN_POINT ( 'NONE',  ( -27.00000000000000000, 43.00000000000000000, 11.99999999999999645 ) ) ;
#8221 = CARTESIAN_POINT ( 'NONE',  ( 60.00000000000000000, -3.673940397442057600E-15, -70.00000000000000000 ) ) ;
#8222 = EDGE_LOOP ( 'NONE', ( #8388, #7214 ) ) ;
#8223 = CARTESIAN_POINT ( 'NONE',  ( 27.00000000000000000, -43.00000000000000000, 11.99999999999999645 ) ) ;
#8224 = EDGE_LOOP ( 'NONE', ( #4425, #6555, #2928, #5405 ) ) ;
#8225 = AXIS2_PLACEMENT_3D ( 'NONE', #3169, #6738, #6062 ) ;
#8226 = LINE ( 'NONE', #9129, #495 ) ;
#8227 = CARTESIAN_POINT ( 'NONE',  ( 5.000000000000000000, 9.603694566548697359E-13, 20.00000000000290612 ) ) ;
#8228 = CARTESIAN_POINT ( 'NONE',  ( 17.50000000000000355, 0.000000000000000000, 0.000000000000000000 ) ) ;
#8229 = EDGE_CURVE ( 'NONE', #8147, #3234, #1033, .T. ) ;
#8230 = CIRCLE ( 'NONE', #6697, 0.7500000000012114754 ) ;
#8231 = EDGE_CURVE ( 'NONE', #672, #5549, #401, .T. ) ;
#8232 = VECTOR ( 'NONE', #3925, 1000.000000000000000 ) ;
#8233 = EDGE_LOOP ( 'NONE', ( #1480, #5187, #4337, #7332, #8190, #1506 ) ) ;
#8234 = ADVANCED_FACE ( 'NONE', ( #5372, #3973 ), #6855, .T. ) ;
#8235 = ADVANCED_FACE ( 'NONE', ( #1707 ), #1168, .T. ) ;
#8236 = EDGE_LOOP ( 'NONE', ( #7088, #5287 ) ) ;
#8237 = VERTEX_POINT ( 'NONE', #6804 ) ;
#8238 = EDGE_LOOP ( 'NONE', ( #5137, #3503 ) ) ;
#8239 = LINE ( 'NONE', #3969, #6130 ) ;
#8240 = CARTESIAN_POINT ( 'NONE',  ( -0.7500000000000000000, 2.750000000000002665, 1.500000000000000000 ) ) ;
#8241 = LINE ( 'NONE', #7373, #1017 ) ;
#8242 = VECTOR ( 'NONE', #3761, 1000.000000000000000 ) ;
#8243 = EDGE_CURVE ( 'NONE', #23, #8998, #8837, .T. ) ;
#8244 = DIRECTION ( 'NONE',  ( -1.000000000000000000, 0.000000000000000000, 0.000000000000000000 ) ) ;
#8245 = AXIS2_PLACEMENT_3D ( 'NONE', #1985, #4909, #9323 ) ;
#8246 = CARTESIAN_POINT ( 'NONE',  ( 2.143131898507868248E-15, -17.50000000000000000, 14.49999999999999822 ) ) ;
#8247 = ADVANCED_FACE ( 'NONE', ( #981 ), #6865, .F. ) ;
#8248 = DIRECTION ( 'NONE',  ( 0.000000000000000000, 0.000000000000000000, -1.000000000000000000 ) ) ;
#8249 = VECTOR ( 'NONE', #7285, 1000.000000000000000 ) ;
#8250 = DIRECTION ( 'NONE',  ( -0.000000000000000000, -0.000000000000000000, -1.000000000000000000 ) ) ;
#8251 = EDGE_CURVE ( 'NONE', #424, #4140, #7776, .T. ) ;
#8252 = AXIS2_PLACEMENT_3D ( 'NONE', #4810, #3414, #5000 ) ;
#8253 = ORIENTED_EDGE ( 'NONE', *, *, #6963, .T. ) ;
#8254 = VERTEX_POINT ( 'NONE', #4915 ) ;
#8255 = DIRECTION ( 'NONE',  ( 0.000000000000000000, 0.000000000000000000, -1.000000000000000000 ) ) ;
#8256 = EDGE_LOOP ( 'NONE', ( #3474, #4080, #2020, #9149 ) ) ;
#8257 = EDGE_CURVE ( 'NONE', #5235, #3097, #4196, .T. ) ;
#8258 = VECTOR ( 'NONE', #4655, 999.9999999999998863 ) ;
#8259 = CARTESIAN_POINT ( 'NONE',  ( 6.000000000000000888, 22.50000000000000355, 5.000000000000000000 ) ) ;
#8260 = ORIENTED_EDGE ( 'NONE', *, *, #5424, .F. ) ;
#8261 = CARTESIAN_POINT ( 'NONE',  ( 0.6691251631324991456, 28.75033890800110825, 1.750217869429287365 ) ) ;
#8262 = AXIS2_PLACEMENT_3D ( 'NONE', #7532, #2497, #5422 ) ;
#8263 = CARTESIAN_POINT ( 'NONE',  ( 27.00000000000000000, 43.00000000000000000, 11.99999999999999645 ) ) ;
#8264 = CARTESIAN_POINT ( 'NONE',  ( 0.000000000000000000, -20.00000000000120437, 1.560000000004989174 ) ) ;
#8265 = ORIENTED_EDGE ( 'NONE', *, *, #8993, .T. ) ;
#8266 = ORIENTED_EDGE ( 'NONE', *, *, #6926, .F. ) ;
#8267 = DIRECTION ( 'NONE',  ( -2.532696274926138358E-16, 0.9997175446104181740, -0.02376617340079587720 ) ) ;
#8268 = DIRECTION ( 'NONE',  ( 0.000000000000000000, 0.000000000000000000, 1.000000000000000000 ) ) ;
#8269 = CARTESIAN_POINT ( 'NONE',  ( 0.000000000000000000, -30.00000000000000000, 0.000000000000000000 ) ) ;
#8270 = CARTESIAN_POINT ( 'NONE',  ( -16.49999999999999645, -7.782354204448209592E-14, 0.000000000000000000 ) ) ;
#8271 = CARTESIAN_POINT ( 'NONE',  ( 60.00000000000000000, 15.90990257669733943, -82.90990257669729147 ) ) ;
#8272 = CYLINDRICAL_SURFACE ( 'NONE', #5051, 30.00000000000000000 ) ;
#8273 = DIRECTION ( 'NONE',  ( -0.000000000000000000, -0.000000000000000000, 1.000000000000000000 ) ) ;
#8274 = ADVANCED_FACE ( 'NONE', ( #5601 ), #558, .T. ) ;
#8275 = ORIENTED_EDGE ( 'NONE', *, *, #5948, .F. ) ;
#8276 = PRESENTATION_STYLE_ASSIGNMENT (( #5300 ) ) ;
#8277 = VERTEX_POINT ( 'NONE', #3569 ) ;
#8278 = DIRECTION ( 'NONE',  ( -0.000000000000000000, 1.000000000000000000, 0.000000000000000000 ) ) ;
#8279 = DIRECTION ( 'NONE',  ( -1.000000000000000000, 0.000000000000000000, -0.000000000000000000 ) ) ;
#8280 = DIRECTION ( 'NONE',  ( 0.000000000000000000, -0.7071067811865472397, -0.7071067811865479058 ) ) ;
#8281 = FACE_OUTER_BOUND ( 'NONE', #3168, .T. ) ;
#8282 = EDGE_LOOP ( 'NONE', ( #6655, #6363, #1040, #9241 ) ) ;
#8283 = ORIENTED_EDGE ( 'NONE', *, *, #4225, .T. ) ;
#8284 = VERTEX_POINT ( 'NONE', #3425 ) ;
#8285 = EDGE_LOOP ( 'NONE', ( #5566, #1924, #7317, #7458, #2764, #52 ) ) ;
#8286 = CARTESIAN_POINT ( 'NONE',  ( -52.42476942962461095, -29.19763577280653877, -80.99738777760511255 ) ) ;
#8287 = CARTESIAN_POINT ( 'NONE',  ( -50.79490495164537833, 12.50000000000000000, -100.0000000000000000 ) ) ;
#8288 = DIRECTION ( 'NONE',  ( 0.000000000000000000, 0.000000000000000000, -1.000000000000000000 ) ) ;
#8289 = ADVANCED_FACE ( 'NONE', ( #9278 ), #7122, .F. ) ;
#8290 = EDGE_CURVE ( 'NONE', #6850, #31, #8664, .T. ) ;
#8291 = PLANE ( 'NONE',  #7372 ) ;
#8292 = DIRECTION ( 'NONE',  ( -1.000000000000000000, 0.000000000000000000, -0.000000000000000000 ) ) ;
#8293 = CARTESIAN_POINT ( 'NONE',  ( -1.749999999999997780, 1.750000000000013101, 0.000000000000000000 ) ) ;
#8294 = ORIENTED_EDGE ( 'NONE', *, *, #2433, .T. ) ;
#8295 = ORIENTED_EDGE ( 'NONE', *, *, #7231, .T. ) ;
#8296 = DIRECTION ( 'NONE',  ( -0.000000000000000000, -0.000000000000000000, 1.000000000000000000 ) ) ;
#8297 = CIRCLE ( 'NONE', #2780, 15.00000000000000000 ) ;
#8298 = ORIENTED_EDGE ( 'NONE', *, *, #3547, .T. ) ;
#8299 = EDGE_CURVE ( 'NONE', #4913, #2936, #1005, .T. ) ;
#8300 = LINE ( 'NONE', #4651, #2625 ) ;
#8301 = VERTEX_POINT ( 'NONE', #4870 ) ;
#8302 = DIRECTION ( 'NONE',  ( -1.000000000000000000, -0.000000000000000000, -0.000000000000000000 ) ) ;
#8303 = EDGE_CURVE ( 'NONE', #804, #3622, #7894, .T. ) ;
#8304 = AXIS2_PLACEMENT_3D ( 'NONE', #7566, #317, #9096 ) ;
#8305 = FACE_OUTER_BOUND ( 'NONE', #4350, .T. ) ;
#8306 = CARTESIAN_POINT ( 'NONE',  ( 25.50000000000000355, 2.360423844116556880E-13, 5.000000000000000000 ) ) ;
#8307 = ORIENTED_EDGE ( 'NONE', *, *, #7404, .F. ) ;
#8308 = ORIENTED_EDGE ( 'NONE', *, *, #7810, .T. ) ;
#8309 = LINE ( 'NONE', #1730, #3935 ) ;
#8310 = DIRECTION ( 'NONE',  ( -1.000000000000000000, -0.000000000000000000, -0.000000000000000000 ) ) ;
#8311 = CIRCLE ( 'NONE', #9075, 1.560000000002327303 ) ;
#8312 = PLANE ( 'NONE',  #7126 ) ;
#8313 = CARTESIAN_POINT ( 'NONE',  ( 5.000000000000000000, -18.47759065022712832, 7.653668647304757044 ) ) ;
#8314 = LINE ( 'NONE', #6929, #1427 ) ;
#8315 = ORIENTED_EDGE ( 'NONE', *, *, #5242, .F. ) ;
#8316 = CARTESIAN_POINT ( 'NONE',  ( -19.50000000000000355, 3.673940397442054445E-16, 10.00000000000000000 ) ) ;
#8317 = ORIENTED_EDGE ( 'NONE', *, *, #2191, .F. ) ;
#8318 = CARTESIAN_POINT ( 'NONE',  ( -31.99999999999999289, -34.99999999999999289, 5.000000000000004441 ) ) ;
#8319 = CARTESIAN_POINT ( 'NONE',  ( -15.00000000000000000, 0.000000000000000000, 27.50000000000000355 ) ) ;
#8320 = VECTOR ( 'NONE', #6454, 1000.000000000000000 ) ;
#8321 = FACE_OUTER_BOUND ( 'NONE', #8378, .T. ) ;
#8322 = EDGE_CURVE ( 'NONE', #7179, #9313, #7196, .T. ) ;
#8323 = LINE ( 'NONE', #4775, #3398 ) ;
#8324 = ORIENTED_EDGE ( 'NONE', *, *, #7702, .F. ) ;
#8325 = VERTEX_POINT ( 'NONE', #4242 ) ;
#8326 = EDGE_CURVE ( 'NONE', #7366, #6094, #9380, .T. ) ;
#8327 = ORIENTED_EDGE ( 'NONE', *, *, #8618, .F. ) ;
#8328 = AXIS2_PLACEMENT_3D ( 'NONE', #4152, #2623, #6464 ) ;
#8329 = ORIENTED_EDGE ( 'NONE', *, *, #2315, .T. ) ;
#8330 = CYLINDRICAL_SURFACE ( 'NONE', #2551, 3.000000000000002665 ) ;
#8331 = DIRECTION ( 'NONE',  ( 1.224646799147353207E-16, 1.000000000000000000, -0.000000000000000000 ) ) ;
#8332 = CARTESIAN_POINT ( 'NONE',  ( -22.50000000000000355, 0.000000000000000000, 2.000000000000039080 ) ) ;
#8333 = DIRECTION ( 'NONE',  ( 0.000000000000000000, 0.000000000000000000, -1.000000000000000000 ) ) ;
#8334 = CARTESIAN_POINT ( 'NONE',  ( 28.14436749771988033, 2.074924133079033339, 1.218150816307271178 ) ) ;
#8335 = VECTOR ( 'NONE', #3270, 1000.000000000000000 ) ;
#8336 = DIRECTION ( 'NONE',  ( -0.000000000000000000, -0.000000000000000000, -1.000000000000000000 ) ) ;
#8337 = ORIENTED_EDGE ( 'NONE', *, *, #7543, .F. ) ;
#8338 = EDGE_LOOP ( 'NONE', ( #6210, #8466, #3612, #7047, #6610, #4807 ) ) ;
#8339 = DIRECTION ( 'NONE',  ( 1.000000000000000000, 0.000000000000000000, 0.000000000000000000 ) ) ;
#8340 = VERTEX_POINT ( 'NONE', #6466 ) ;
#8341 = DIRECTION ( 'NONE',  ( 0.000000000000000000, 0.000000000000000000, 1.000000000000000000 ) ) ;
#8342 = CARTESIAN_POINT ( 'NONE',  ( 0.000000000000000000, 34.00000000000001421, 32.00000000000000000 ) ) ;
#8343 = ORIENTED_EDGE ( 'NONE', *, *, #6711, .F. ) ;
#8344 = CARTESIAN_POINT ( 'NONE',  ( 4.000000000000000000, -18.47759065022790637, -7.653668647299759265 ) ) ;
#8345 = ADVANCED_FACE ( 'NONE', ( #2806 ), #5745, .T. ) ;
#8346 = EDGE_CURVE ( 'NONE', #2860, #5108, #1215, .T. ) ;
#8347 = ADVANCED_FACE ( 'NONE', ( #4107 ), #9428, .F. ) ;
#8348 = DIRECTION ( 'NONE',  ( -0.000000000000000000, -0.000000000000000000, -1.000000000000000000 ) ) ;
#8349 = DIRECTION ( 'NONE',  ( -1.000000000000000000, 0.000000000000000000, 0.000000000000000000 ) ) ;
#8350 = ORIENTED_EDGE ( 'NONE', *, *, #2959, .F. ) ;
#8351 = CIRCLE ( 'NONE', #377, 1.560000000002236709 ) ;
#8352 = ORIENTED_EDGE ( 'NONE', *, *, #4232, .F. ) ;
#8353 = EDGE_CURVE ( 'NONE', #4159, #7855, #9004, .T. ) ;
#8354 = ITEM_DEFINED_TRANSFORMATION ( 'NONE', 'NONE', #7907,  #1614 ) ;
#8355 = CARTESIAN_POINT ( 'NONE',  ( -51.96152422706632024, -30.00000000000000000, -13.00000000000000000 ) ) ;
#8356 = CIRCLE ( 'NONE', #8666, 6.000000000000000000 ) ;
#8357 = ADVANCED_FACE ( 'NONE', ( #2221 ), #5878, .F. ) ;
#8358 =( BOUNDED_CURVE ( )  B_SPLINE_CURVE ( 3, ( #3710, #4381, #2852, #7309 ),
 .UNSPECIFIED., .F., .T. ) 
 B_SPLINE_CURVE_WITH_KNOTS ( ( 4, 4 ),
 ( 1.570796326794896558, 3.069868295139984049 ),
 .UNSPECIFIED. ) 
 CURVE ( )  GEOMETRIC_REPRESENTATION_ITEM ( )  RATIONAL_B_SPLINE_CURVE ( ( 1.000000000000000000, 0.8213367208436757050, 0.8213367208436757050, 1.000000000000000000 ) ) 
 REPRESENTATION_ITEM ( '' )  );
#8359 = APPLICATION_CONTEXT ( 'automotive_design' ) ;
#8360 = CARTESIAN_POINT ( 'NONE',  ( 27.00000000000000355, 35.00000000000000000, 64.00000000000000000 ) ) ;
#8361 = SURFACE_SIDE_STYLE ('',( #2555 ) ) ;
#8362 = DIRECTION ( 'NONE',  ( 0.7071067811865486830, 8.659560562354948882E-17, -0.7071067811865464625 ) ) ;
#8363 = EDGE_CURVE ( 'NONE', #9459, #2492, #1955, .T. ) ;
#8364 = DIRECTION ( 'NONE',  ( -1.000000000000000000, 0.000000000000000000, 0.000000000000000000 ) ) ;
#8365 = EDGE_CURVE ( 'NONE', #1286, #6850, #5937, .T. ) ;
#8366 = EDGE_LOOP ( 'NONE', ( #7096, #4025 ) ) ;
#8367 = DIRECTION ( 'NONE',  ( 0.000000000000000000, 1.000000000000000000, 0.000000000000000000 ) ) ;
#8368 = ORIENTED_EDGE ( 'NONE', *, *, #3015, .F. ) ;
#8369 = EDGE_CURVE ( 'NONE', #2908, #7012, #8036, .T. ) ;
#8370 = CARTESIAN_POINT ( 'NONE',  ( 4.000000000000000000, -18.47759065022712832, 8.403668647304948891 ) ) ;
#8371 = DIRECTION ( 'NONE',  ( 1.000000000000000000, 0.000000000000000000, 0.000000000000000000 ) ) ;
#8372 = VERTEX_POINT ( 'NONE', #7999 ) ;
#8373 = FACE_OUTER_BOUND ( 'NONE', #6702, .T. ) ;
#8374 = DIRECTION ( 'NONE',  ( -1.000000000000000000, 0.000000000000000000, 0.000000000000000000 ) ) ;
#8375 = ORIENTED_EDGE ( 'NONE', *, *, #9280, .T. ) ;
#8376 = ORIENTED_EDGE ( 'NONE', *, *, #56, .T. ) ;
#8377 = AXIS2_PLACEMENT_3D ( 'NONE', #10, #2929, #7253 ) ;
#8378 = EDGE_LOOP ( 'NONE', ( #6898, #8308, #5795, #3639 ) ) ;
#8379 =( NAMED_UNIT ( * ) PLANE_ANGLE_UNIT ( ) SI_UNIT ( $, .RADIAN. ) );
#8380 = ORIENTED_EDGE ( 'NONE', *, *, #2177, .F. ) ;
#8381 = CARTESIAN_POINT ( 'NONE',  ( -27.00000000000000000, -43.00000000000000000, 25.00000000000000000 ) ) ;
#8382 = DIRECTION ( 'NONE',  ( 0.000000000000000000, -1.224646799147353454E-16, 1.000000000000000000 ) ) ;
#8383 = CARTESIAN_POINT ( 'NONE',  ( 16.00000000000000000, -43.00000000000000000, -7.366666666666667140 ) ) ;
#8384 = CARTESIAN_POINT ( 'NONE',  ( -41.99999999999999289, 12.50000000000000000, -100.0000000000000000 ) ) ;
#8385 = VECTOR ( 'NONE', #2767, 1000.000000000000000 ) ;
#8386 = CARTESIAN_POINT ( 'NONE',  ( -37.22467645238198486, 47.05659850664388699, -5.608807313787648852 ) ) ;
#8387 = CARTESIAN_POINT ( 'NONE',  ( 28.48969330601476813, -2.327370969396562295, 1.582659982438076263 ) ) ;
#8388 = ORIENTED_EDGE ( 'NONE', *, *, #9460, .T. ) ;
#8389 = ORIENTED_EDGE ( 'NONE', *, *, #5371, .T. ) ;
#8390 = EDGE_CURVE ( 'NONE', #4790, #6148, #4403, .T. ) ;
#8391 = DIRECTION ( 'NONE',  ( -1.000000000000000000, -0.000000000000000000, -0.000000000000000000 ) ) ;
#8392 = ORIENTED_EDGE ( 'NONE', *, *, #4456, .F. ) ;
#8393 = AXIS2_PLACEMENT_3D ( 'NONE', #5833, #1452, #4481 ) ;
#8394 = CARTESIAN_POINT ( 'NONE',  ( 39.50000000000000000, 29.99999999999999645, -82.50000000000000000 ) ) ;
#8395 = FACE_OUTER_BOUND ( 'NONE', #8256, .T. ) ;
#8396 = ORIENTED_EDGE ( 'NONE', *, *, #7020, .T. ) ;
#8397 = CIRCLE ( 'NONE', #7470, 3.000000000000002665 ) ;
#8398 = DIRECTION ( 'NONE',  ( 1.000000000000000000, 0.000000000000000000, 0.000000000000000000 ) ) ;
#8399 = CONICAL_SURFACE ( 'NONE', #4251, 6.000000000000001776, 0.7853981633974431720 ) ;
#8400 = CIRCLE ( 'NONE', #568, 7.250000000000002665 ) ;
#8401 = LINE ( 'NONE', #5335, #2831 ) ;
#8402 = DIRECTION ( 'NONE',  ( -0.000000000000000000, -0.000000000000000000, -1.000000000000000000 ) ) ;
#8403 = VECTOR ( 'NONE', #7288, 999.9999999999998863 ) ;
#8404 = ORIENTED_EDGE ( 'NONE', *, *, #7386, .T. ) ;
#8405 = VERTEX_POINT ( 'NONE', #168 ) ;
#8406 = CIRCLE ( 'NONE', #7945, 1.560000000001265263 ) ;
#8407 = SHAPE_DEFINITION_REPRESENTATION ( #4922, #7573 ) ;
#8408 = CONICAL_SURFACE ( 'NONE', #126, 22.00000000000000711, 0.7853981633974482790 ) ;
#8409 = ADVANCED_FACE ( 'NONE', ( #8848 ), #1403, .T. ) ;
#8410 = CARTESIAN_POINT ( 'NONE',  ( 32.00000000000000711, 2.265596578422603791E-15, 50.50000000000000000 ) ) ;
#8411 = EDGE_CURVE ( 'NONE', #2905, #75, #8799, .T. ) ;
#8412 = AXIS2_PLACEMENT_3D ( 'NONE', #5438, #963, #8416 ) ;
#8413 = EDGE_CURVE ( 'NONE', #8953, #7815, #871, .T. ) ;
#8414 = EDGE_CURVE ( 'NONE', #4536, #7086, #1034, .T. ) ;
#8415 = FACE_OUTER_BOUND ( 'NONE', #7461, .T. ) ;
#8416 = DIRECTION ( 'NONE',  ( 0.000000000000000000, 0.000000000000000000, 1.000000000000000000 ) ) ;
#8417 = CARTESIAN_POINT ( 'NONE',  ( 2.143131898507868248E-15, -35.00000000000000000, 14.49999999999999822 ) ) ;
#8418 = DIRECTION ( 'NONE',  ( 1.000000000000000000, 0.000000000000000000, 0.000000000000000000 ) ) ;
#8419 = ORIENTED_EDGE ( 'NONE', *, *, #1838, .F. ) ;
#8420 = CARTESIAN_POINT ( 'NONE',  ( -37.00000000000000711, 15.90990257669733943, -82.90990257669729147 ) ) ;
#8421 = CIRCLE ( 'NONE', #5877, 15.00000000000000000 ) ;
#8422 = AXIS2_PLACEMENT_3D ( 'NONE', #6614, #4306, #8044 ) ;
#8423 = ORIENTED_EDGE ( 'NONE', *, *, #4261, .T. ) ;
#8424 = CIRCLE ( 'NONE', #1842, 3.000000000000002665 ) ;
#8425 = DIRECTION ( 'NONE',  ( 0.000000000000000000, 0.000000000000000000, -1.000000000000000000 ) ) ;
#8426 = EDGE_CURVE ( 'NONE', #85, #4903, #7468, .T. ) ;
#8427 = CARTESIAN_POINT ( 'NONE',  ( 17.50000000000000355, 0.000000000000000000, 1.000000000000021760 ) ) ;
#8428 = DIRECTION ( 'NONE',  ( 1.000000000000000000, 0.000000000000000000, 0.000000000000000000 ) ) ;
#8429 = DIRECTION ( 'NONE',  ( 0.000000000000000000, 0.000000000000000000, 1.000000000000000000 ) ) ;
#8430 = AXIS2_PLACEMENT_3D ( 'NONE', #1012, #2414, #9078 ) ;
#8431 = EDGE_CURVE ( 'NONE', #6279, #2195, #3089, .T. ) ;
#8432 = VECTOR ( 'NONE', #7454, 1000.000000000000114 ) ;
#8433 = EDGE_LOOP ( 'NONE', ( #4279, #8997, #6313 ) ) ;
#8434 = ORIENTED_EDGE ( 'NONE', *, *, #6465, .F. ) ;
#8435 = CARTESIAN_POINT ( 'NONE',  ( 70.51394605043111596, 96.36314398677504300, 59.86606487507483365 ) ) ;
#8436 = VERTEX_POINT ( 'NONE', #1502 ) ;
#8437 = DIRECTION ( 'NONE',  ( -0.000000000000000000, 1.000000000000000000, 1.224646799147353207E-16 ) ) ;
#8438 = EDGE_CURVE ( 'NONE', #8254, #7899, #4385, .T. ) ;
#8439 = DIRECTION ( 'NONE',  ( 0.000000000000000000, -1.000000000000000000, 0.000000000000000000 ) ) ;
#8440 = FACE_OUTER_BOUND ( 'NONE', #6954, .T. ) ;
#8441 = CARTESIAN_POINT ( 'NONE',  ( 28.50000000000001066, 0.2131062308235842917, 1.500000000000043299 ) ) ;
#8442 = CARTESIAN_POINT ( 'NONE',  ( 0.000000000000000000, 0.000000000000000000, 63.00000000000002842 ) ) ;
#8443 = EDGE_LOOP ( 'NONE', ( #2351, #8834, #6902, #2666 ) ) ;
#8444 = ORIENTED_EDGE ( 'NONE', *, *, #2300, .F. ) ;
#8445 = VECTOR ( 'NONE', #3080, 1000.000000000000000 ) ;
#8446 = LINE ( 'NONE', #4604, #6252 ) ;
#8447 = ORIENTED_EDGE ( 'NONE', *, *, #8290, .T. ) ;
#8448 = FACE_BOUND ( 'NONE', #1153, .T. ) ;
#8449 = ORIENTED_EDGE ( 'NONE', *, *, #5010, .F. ) ;
#8450 = LINE ( 'NONE', #2640, #4769 ) ;
#8451 = ADVANCED_FACE ( 'NONE', ( #3617 ), #68, .F. ) ;
#8452 = DIRECTION ( 'NONE',  ( -1.000000000000000000, 0.000000000000000000, 0.000000000000000000 ) ) ;
#8453 = AXIS2_PLACEMENT_3D ( 'NONE', #2867, #1923, #5759 ) ;
#8454 = CYLINDRICAL_SURFACE ( 'NONE', #8711, 6.000000000000000888 ) ;
#8455 = ORIENTED_EDGE ( 'NONE', *, *, #3222, .T. ) ;
#8456 = ORIENTED_EDGE ( 'NONE', *, *, #7515, .F. ) ;
#8457 = ADVANCED_FACE ( 'NONE', ( #2173, #1599 ), #8139, .T. ) ;
#8458 = CONTEXT_DEPENDENT_SHAPE_REPRESENTATION ( #3266, #7917 ) ;
#8459 = VECTOR ( 'NONE', #5460, 1000.000000000000000 ) ;
#8460 = CARTESIAN_POINT ( 'NONE',  ( 0.000000000000000000, 0.000000000000000000, 0.000000000000000000 ) ) ;
#8461 = DIRECTION ( 'NONE',  ( -0.7071067811865500152, 0.000000000000000000, 0.7071067811865451302 ) ) ;
#8462 = CARTESIAN_POINT ( 'NONE',  ( 0.000000000000000000, 0.000000000000000000, 1.000000000000000000 ) ) ;
#8463 = DIRECTION ( 'NONE',  ( -0.7071067811865494601, 0.7071067811865455743, 0.000000000000000000 ) ) ;
#8464 = VERTEX_POINT ( 'NONE', #821 ) ;
#8465 = LINE ( 'NONE', #5537, #277 ) ;
#8466 = ORIENTED_EDGE ( 'NONE', *, *, #1731, .T. ) ;
#8467 = LINE ( 'NONE', #1291, #6795 ) ;
#8468 = CONICAL_SURFACE ( 'NONE', #3093, 17.50000000000000355, 0.7853981633974533860 ) ;
#8469 = FACE_OUTER_BOUND ( 'NONE', #1759, .T. ) ;
#8470 = DIRECTION ( 'NONE',  ( 0.000000000000000000, 0.000000000000000000, 1.000000000000000000 ) ) ;
#8471 = ADVANCED_FACE ( 'NONE', ( #5105 ), #6694, .T. ) ;
#8472 = DIRECTION ( 'NONE',  ( -1.000000000000000000, -0.000000000000000000, -0.000000000000000000 ) ) ;
#8473 = ADVANCED_FACE ( 'NONE', ( #7453 ), #875, .F. ) ;
#8474 = LINE ( 'NONE', #7031, #7783 ) ;
#8475 = VECTOR ( 'NONE', #2212, 1000.000000000000000 ) ;
#8476 = ORIENTED_EDGE ( 'NONE', *, *, #7823, .T. ) ;
#8477 = ORIENTED_EDGE ( 'NONE', *, *, #6926, .T. ) ;
#8478 = CARTESIAN_POINT ( 'NONE',  ( -8.230900400053766219, 144.1190101173697542, 58.80419905176558615 ) ) ;
#8479 = ORIENTED_EDGE ( 'NONE', *, *, #6483, .T. ) ;
#8480 = FACE_OUTER_BOUND ( 'NONE', #2472, .T. ) ;
#8481 = AXIS2_PLACEMENT_3D ( 'NONE', #3411, #4809, #6402 ) ;
#8482 = FACE_OUTER_BOUND ( 'NONE', #6941, .T. ) ;
#8483 = DIRECTION ( 'NONE',  ( 0.000000000000000000, 1.000000000000000000, 0.000000000000000000 ) ) ;
#8484 = CARTESIAN_POINT ( 'NONE',  ( 26.64999999999992752, 4.333301281933056970, 0.000000000000000000 ) ) ;
#8485 = VECTOR ( 'NONE', #9093, 1000.000000000000114 ) ;
#8486 = CARTESIAN_POINT ( 'NONE',  ( 0.7500000000000000000, -0.7500000000000000000, 0.000000000000000000 ) ) ;
#8487 = ORIENTED_EDGE ( 'NONE', *, *, #3230, .F. ) ;
#8488 = ORIENTED_EDGE ( 'NONE', *, *, #8757, .T. ) ;
#8489 = LINE ( 'NONE', #1998, #5330 ) ;
#8490 = ORIENTED_EDGE ( 'NONE', *, *, #8071, .F. ) ;
#8491 = LINE ( 'NONE', #9290, #2123 ) ;
#8492 = CARTESIAN_POINT ( 'NONE',  ( 0.7500000000000000000, -2.750000000000002665, 0.000000000000000000 ) ) ;
#8493 = ORIENTED_EDGE ( 'NONE', *, *, #6545, .F. ) ;
#8494 = DIRECTION ( 'NONE',  ( 0.000000000000000000, 0.000000000000000000, 1.000000000000000000 ) ) ;
#8495 = CARTESIAN_POINT ( 'NONE',  ( 1.571166602479410136E-13, -22.50000000000000355, 5.000000000000000000 ) ) ;
#8496 = AXIS2_PLACEMENT_3D ( 'NONE', #5020, #4967, #7177 ) ;
#8497 = DIRECTION ( 'NONE',  ( -0.000000000000000000, -0.000000000000000000, -1.000000000000000000 ) ) ;
#8498 = ORIENTED_EDGE ( 'NONE', *, *, #2452, .F. ) ;
#8499 = ORIENTED_EDGE ( 'NONE', *, *, #2234, .F. ) ;
#8500 = AXIS2_PLACEMENT_3D ( 'NONE', #2490, #278, #182 ) ;
#8501 = SHAPE_REPRESENTATION ( '6-M6-16', ( #1614 ), #6385 ) ;
#8502 = DIRECTION ( 'NONE',  ( -1.000000000000000000, 0.000000000000000000, -0.000000000000000000 ) ) ;
#8503 = CARTESIAN_POINT ( 'NONE',  ( 50.79490495164537833, 29.99999999999999645, -82.50000000000000000 ) ) ;
#8504 = DIRECTION ( 'NONE',  ( -1.000000000000000000, -0.000000000000000000, -0.000000000000000000 ) ) ;
#8505 = DIRECTION ( 'NONE',  ( 1.000000000000000000, 0.000000000000000000, 0.000000000000000000 ) ) ;
#8506 = ORIENTED_EDGE ( 'NONE', *, *, #6043, .F. ) ;
#8507 = ORIENTED_EDGE ( 'NONE', *, *, #5065, .F. ) ;
#8508 = PRESENTATION_LAYER_ASSIGNMENT (  '', '', ( #5131 ) ) ;
#8509 = ORIENTED_EDGE ( 'NONE', *, *, #7993, .F. ) ;
#8510 = CARTESIAN_POINT ( 'NONE',  ( -0.7500000000000000000, -0.7500000000000000000, 1.500000000000000000 ) ) ;
#8511 = CIRCLE ( 'NONE', #7277, 3.000000000000000444 ) ;
#8512 = PLANE ( 'NONE',  #117 ) ;
#8513 = ADVANCED_FACE ( 'NONE', ( #4726 ), #8843, .F. ) ;
#8514 = DIRECTION ( 'NONE',  ( -0.7071067811865525687, 0.000000000000000000, 0.7071067811865425767 ) ) ;
#8515 = DIRECTION ( 'NONE',  ( 0.000000000000000000, -0.000000000000000000, 1.000000000000000000 ) ) ;
#8516 =( NAMED_UNIT ( * ) PLANE_ANGLE_UNIT ( ) SI_UNIT ( $, .RADIAN. ) );
#8517 = EDGE_LOOP ( 'NONE', ( #9264, #2455, #806, #7988 ) ) ;
#8518 = VERTEX_POINT ( 'NONE', #6794 ) ;
#8519 = VERTEX_POINT ( 'NONE', #3905 ) ;
#8520 = EDGE_CURVE ( 'NONE', #804, #8237, #1508, .T. ) ;
#8521 = VECTOR ( 'NONE', #8966, 1000.000000000000000 ) ;
#8522 = DIRECTION ( 'NONE',  ( -1.000000000000000000, 1.224646799147353454E-16, 0.000000000000000000 ) ) ;
#8523 = DIRECTION ( 'NONE',  ( 0.000000000000000000, 0.000000000000000000, -1.000000000000000000 ) ) ;
#8524 = ADVANCED_FACE ( 'NONE', ( #6983 ), #5400, .F. ) ;
#8525 = DIRECTION ( 'NONE',  ( -1.000000000000000000, -0.000000000000000000, -0.000000000000000000 ) ) ;
#8526 = ADVANCED_FACE ( 'NONE', ( #4583 ), #5496, .F. ) ;
#8527 = DIRECTION ( 'NONE',  ( 1.000000000000000000, 0.000000000000000000, 0.000000000000000000 ) ) ;
#8528 = ADVANCED_FACE ( 'NONE', ( #391 ), #8990, .F. ) ;
#8529 = EDGE_CURVE ( 'NONE', #3983, #85, #3637, .T. ) ;
#8530 = AXIS2_PLACEMENT_3D ( 'NONE', #2926, #7801, #1436 ) ;
#8531 = FACE_OUTER_BOUND ( 'NONE', #3638, .T. ) ;
#8532 = VERTEX_POINT ( 'NONE', #3185 ) ;
#8533 = ORIENTED_EDGE ( 'NONE', *, *, #6304, .F. ) ;
#8534 = LINE ( 'NONE', #1367, #8976 ) ;
#8535 = ORIENTED_EDGE ( 'NONE', *, *, #5657, .T. ) ;
#8536 = DIRECTION ( 'NONE',  ( -3.969829082701935600E-15, -0.7071067811865493491, 0.7071067811865456854 ) ) ;
#8537 = DIRECTION ( 'NONE',  ( 0.000000000000000000, 0.000000000000000000, -1.000000000000000000 ) ) ;
#8538 = LINE ( 'NONE', #2682, #263 ) ;
#8539 = VECTOR ( 'NONE', #2731, 1000.000000000000000 ) ;
#8540 = FACE_OUTER_BOUND ( 'NONE', #254, .T. ) ;
#8541 = EDGE_CURVE ( 'NONE', #7550, #7477, #2376, .T. ) ;
#8542 = CARTESIAN_POINT ( 'NONE',  ( 19.50000000000000355, 2.356749903719115078E-13, 15.00000000000000000 ) ) ;
#8543 = CARTESIAN_POINT ( 'NONE',  ( -39.50000000000000711, 15.00000000000000533, -97.50000000000001421 ) ) ;
#8544 = EDGE_CURVE ( 'NONE', #472, #1561, #721, .T. ) ;
#8545 = VECTOR ( 'NONE', #4293, 1000.000000000000000 ) ;
#8546 = ORIENTED_EDGE ( 'NONE', *, *, #8052, .F. ) ;
#8547 = ORIENTED_EDGE ( 'NONE', *, *, #5830, .T. ) ;
#8548 =( REPRESENTATION_RELATIONSHIP ('NONE','NONE', #1933, #7573 ) REPRESENTATION_RELATIONSHIP_WITH_TRANSFORMATION ( #3993 )SHAPE_REPRESENTATION_RELATIONSHIP( ) );
#8549 = DIRECTION ( 'NONE',  ( 1.000000000000000000, 1.776356839400250465E-15, 0.000000000000000000 ) ) ;
#8550 = CARTESIAN_POINT ( 'NONE',  ( -37.22467645238198486, 47.05659850664388699, -5.608807313787648852 ) ) ;
#8551 = DIRECTION ( 'NONE',  ( 0.000000000000000000, 0.000000000000000000, 1.000000000000000000 ) ) ;
#8552 = AXIS2_PLACEMENT_3D ( 'NONE', #2017, #1922, #9363 ) ;
#8553 = ORIENTED_EDGE ( 'NONE', *, *, #3547, .F. ) ;
#8554 = ORIENTED_EDGE ( 'NONE', *, *, #3471, .F. ) ;
#8555 = ORIENTED_EDGE ( 'NONE', *, *, #5772, .T. ) ;
#8556 = VECTOR ( 'NONE', #9029, 1000.000000000000000 ) ;
#8557 = ORIENTED_EDGE ( 'NONE', *, *, #5129, .T. ) ;
#8558 = DIRECTION ( 'NONE',  ( 0.000000000000000000, 0.000000000000000000, -1.000000000000000000 ) ) ;
#8559 = AXIS2_PLACEMENT_3D ( 'NONE', #8342, #2539, #4700 ) ;
#8560 = DIRECTION ( 'NONE',  ( -1.000000000000000000, 0.000000000000000000, -0.000000000000000000 ) ) ;
#8561 = DIRECTION ( 'NONE',  ( 0.000000000000000000, 0.000000000000000000, -1.000000000000000000 ) ) ;
#8562 = DIRECTION ( 'NONE',  ( 1.000000000000000000, -0.000000000000000000, -0.000000000000000000 ) ) ;
#8563 = EDGE_CURVE ( 'NONE', #2915, #6915, #1327, .T. ) ;
#8564 = DIRECTION ( 'NONE',  ( 0.000000000000000000, 0.000000000000000000, 1.000000000000000000 ) ) ;
#8565 = VECTOR ( 'NONE', #4450, 1000.000000000000000 ) ;
#8566 = VERTEX_POINT ( 'NONE', #8427 ) ;
#8567 = ORIENTED_EDGE ( 'NONE', *, *, #4548, .T. ) ;
#8568 = DIRECTION ( 'NONE',  ( 0.000000000000000000, -0.5535840618632023036, -0.8327933035579949683 ) ) ;
#8569 = ORIENTED_EDGE ( 'NONE', *, *, #5542, .F. ) ;
#8570 = DIRECTION ( 'NONE',  ( 1.000000000000000000, 0.000000000000000000, 0.000000000000000000 ) ) ;
#8571 = EDGE_CURVE ( 'NONE', #3040, #3178, #259, .T. ) ;
#8572 = CARTESIAN_POINT ( 'NONE',  ( -60.00000000000000000, -30.00000000000000000, -13.00000000000000000 ) ) ;
#8573 = CIRCLE ( 'NONE', #8422, 22.50000000000000000 ) ;
#8574 = CARTESIAN_POINT ( 'NONE',  ( 38.00000000000000000, 43.00000000000000000, -7.366666666666667140 ) ) ;
#8575 = CIRCLE ( 'NONE', #4750, 15.00000000000000000 ) ;
#8576 = DIRECTION ( 'NONE',  ( 1.000000000000000000, 0.000000000000000000, 0.000000000000000000 ) ) ;
#8577 = CARTESIAN_POINT ( 'NONE',  ( 27.00000000000000355, -29.99999999999999289, 64.00000000000000000 ) ) ;
#8578 = ORIENTED_EDGE ( 'NONE', *, *, #6522, .T. ) ;
#8579 = ORIENTED_EDGE ( 'NONE', *, *, #310, .T. ) ;
#8580 = CARTESIAN_POINT ( 'NONE',  ( -3.168636005458878024, 27.60958896060101964, 0.7887504010224319906 ) ) ;
#8581 = ORIENTED_EDGE ( 'NONE', *, *, #6878, .F. ) ;
#8582 = CARTESIAN_POINT ( 'NONE',  ( -28.75000000000002132, 2.329604860730800488E-26, 1.750000000000023537 ) ) ;
#8583 = DIRECTION ( 'NONE',  ( 0.000000000000000000, 0.000000000000000000, 1.000000000000000000 ) ) ;
#8584 = CARTESIAN_POINT ( 'NONE',  ( 32.00000000000000711, 35.00000000000000000, 5.000000000000031974 ) ) ;
#8585 = DIRECTION ( 'NONE',  ( -0.000000000000000000, -0.000000000000000000, -1.000000000000000000 ) ) ;
#8586 = LINE ( 'NONE', #2005, #373 ) ;
#8587 = LINE ( 'NONE', #2781, #3959 ) ;
#8588 = EDGE_CURVE ( 'NONE', #4625, #2573, #8091, .T. ) ;
#8589 = ORIENTED_EDGE ( 'NONE', *, *, #8251, .F. ) ;
#8590 = EDGE_LOOP ( 'NONE', ( #8902, #7450, #5406, #6998, #515 ) ) ;
#8591 = CONTEXT_DEPENDENT_SHAPE_REPRESENTATION ( #5232, #6625 ) ;
#8592 = CARTESIAN_POINT ( 'NONE',  ( -31.99999999999999289, 2.265596578422605368E-15, 13.49999999999998401 ) ) ;
#8593 = CARTESIAN_POINT ( 'NONE',  ( 32.00000000000000711, -34.99999999999999289, 5.000000000000031974 ) ) ;
#8594 = CYLINDRICAL_SURFACE ( 'NONE', #6962, 2.999999999999999556 ) ;
#8595 = CARTESIAN_POINT ( 'NONE',  ( -26.99999999999998934, -34.99999999999999289, 58.99999999999997158 ) ) ;
#8596 = ORIENTED_EDGE ( 'NONE', *, *, #3296, .T. ) ;
#8597 = ORIENTED_EDGE ( 'NONE', *, *, #462, .F. ) ;
#8598 = ORIENTED_EDGE ( 'NONE', *, *, #4943, .T. ) ;
#8599 = CIRCLE ( 'NONE', #4463, 3.000000000000002665 ) ;
#8600 = ORIENTED_EDGE ( 'NONE', *, *, #5675, .T. ) ;
#8601 = DIRECTION ( 'NONE',  ( 0.000000000000000000, 0.000000000000000000, -1.000000000000000000 ) ) ;
#8602 = CYLINDRICAL_SURFACE ( 'NONE', #2877, 11.00000000000000711 ) ;
#8603 = LINE ( 'NONE', #7840, #5044 ) ;
#8604 = PRODUCT_DEFINITION_SHAPE ( 'NONE', 'NONE',  #9475 ) ;
#8605 = CARTESIAN_POINT ( 'NONE',  ( 0.000000000000000000, 0.000000000000000000, 50.00000000000000000 ) ) ;
#8606 = DIRECTION ( 'NONE',  ( 0.000000000000000000, 0.7071067811865494601, -0.7071067811865455743 ) ) ;
#8607 = ORIENTED_EDGE ( 'NONE', *, *, #8116, .T. ) ;
#8608 = EDGE_LOOP ( 'NONE', ( #8901, #1399, #7879, #857, #4558, #3713 ) ) ;
#8609 = DIRECTION ( 'NONE',  ( 1.000000000000000000, 0.000000000000000000, 0.000000000000000000 ) ) ;
#8610 = VERTEX_POINT ( 'NONE', #6842 ) ;
#8611 = AXIS2_PLACEMENT_3D ( 'NONE', #3091, #739, #6030 ) ;
#8612 = CARTESIAN_POINT ( 'NONE',  ( -26.21170834203230982, -53.97171801779368394, -0.5000000000000038858 ) ) ;
#8613 = CARTESIAN_POINT ( 'NONE',  ( -28.26575725008335027, 1.673027373762006054, 1.314514334795903183 ) ) ;
#8614 = EDGE_CURVE ( 'NONE', #1485, #1115, #4712, .T. ) ;
#8615 = LINE ( 'NONE', #5699, #8907 ) ;
#8616 = DIRECTION ( 'NONE',  ( 0.000000000000000000, 0.000000000000000000, 1.000000000000000000 ) ) ;
#8617 = AXIS2_PLACEMENT_3D ( 'NONE', #727, #2267, #102 ) ;
#8618 = EDGE_CURVE ( 'NONE', #8070, #3385, #7927, .T. ) ;
#8619 = DIRECTION ( 'NONE',  ( -0.000000000000000000, -0.000000000000000000, -1.000000000000000000 ) ) ;
#8620 = ORIENTED_EDGE ( 'NONE', *, *, #5542, .T. ) ;
#8621 = EDGE_LOOP ( 'NONE', ( #8533, #2585 ) ) ;
#8622 = CARTESIAN_POINT ( 'NONE',  ( -1.072052546109382609, 28.40723195920987720, 1.426690145881925220 ) ) ;
#8623 = ORIENTED_EDGE ( 'NONE', *, *, #7060, .F. ) ;
#8624 = FACE_OUTER_BOUND ( 'NONE', #797, .T. ) ;
#8625 = CARTESIAN_POINT ( 'NONE',  ( -29.49999999999998224, 29.99999999999997513, 2.500000000000006661 ) ) ;
#8626 = CARTESIAN_POINT ( 'NONE',  ( -27.00000000000000000, -43.00000000000000000, -25.00000000000000000 ) ) ;
#8627 = DIRECTION ( 'NONE',  ( -1.000000000000000000, 0.000000000000000000, -0.000000000000000000 ) ) ;
#8628 = CIRCLE ( 'NONE', #4645, 0.7500000000000006661 ) ;
#8629 = EDGE_CURVE ( 'NONE', #5958, #9178, #6126, .T. ) ;
#8630 = DIRECTION ( 'NONE',  ( -0.000000000000000000, -0.000000000000000000, -1.000000000000000000 ) ) ;
#8631 = CARTESIAN_POINT ( 'NONE',  ( -5.373124232108025033, -27.28744256482707087, 0.8097845059602708506 ) ) ;
#8632 = ORIENTED_EDGE ( 'NONE', *, *, #633, .T. ) ;
#8633 = ORIENTED_EDGE ( 'NONE', *, *, #3953, .T. ) ;
#8634 = DIRECTION ( 'NONE',  ( -1.000000000000000000, 0.000000000000000000, -0.000000000000000000 ) ) ;
#8635 = ITEM_DEFINED_TRANSFORMATION ( 'NONE', 'NONE', #3308,  #1614 ) ;
#8636 = CIRCLE ( 'NONE', #9094, 2.499999999999998668 ) ;
#8637 = EDGE_CURVE ( 'NONE', #900, #55, #4004, .T. ) ;
#8638 = LINE ( 'NONE', #8592, #8403 ) ;
#8639 = EDGE_CURVE ( 'NONE', #3779, #2772, #4679, .T. ) ;
#8640 = EDGE_CURVE ( 'NONE', #2987, #9037, #2248, .T. ) ;
#8641 = CARTESIAN_POINT ( 'NONE',  ( -16.00000000000000000, 1.959434878635765131E-15, 9.999999999999998224 ) ) ;
#8642 = ADVANCED_FACE ( 'NONE', ( #9130 ), #3322, .T. ) ;
#8643 = EDGE_CURVE ( 'NONE', #8518, #3622, #2660, .T. ) ;
#8644 = DIRECTION ( 'NONE',  ( 0.000000000000000000, 0.000000000000000000, -1.000000000000000000 ) ) ;
#8645 = EDGE_LOOP ( 'NONE', ( #1569, #8633, #3316, #969 ) ) ;
#8646 = VECTOR ( 'NONE', #3383, 1000.000000000000000 ) ;
#8647 = ORIENTED_EDGE ( 'NONE', *, *, #5844, .F. ) ;
#8648 = ORIENTED_EDGE ( 'NONE', *, *, #2127, .T. ) ;
#8649 = ORIENTED_EDGE ( 'NONE', *, *, #9396, .F. ) ;
#8650 = CARTESIAN_POINT ( 'NONE',  ( 0.000000000000000000, 0.000000000000000000, 0.000000000000000000 ) ) ;
#8651 = EDGE_CURVE ( 'NONE', #9413, #7367, #1248, .T. ) ;
#8652 = DIRECTION ( 'NONE',  ( 0.000000000000000000, 0.000000000000000000, -1.000000000000000000 ) ) ;
#8653 = CARTESIAN_POINT ( 'NONE',  ( 0.000000000000000000, 0.000000000000000000, 23.99999999999998579 ) ) ;
#8654 = ADVANCED_FACE ( 'NONE', ( #6455 ), #2613, .F. ) ;
#8655 = CYLINDRICAL_SURFACE ( 'NONE', #6327, 1.560000000002236709 ) ;
#8656 = CIRCLE ( 'NONE', #825, 0.7499999999982936982 ) ;
#8657 = FACE_OUTER_BOUND ( 'NONE', #2645, .T. ) ;
#8658 = EDGE_CURVE ( 'NONE', #5932, #2310, #4321, .T. ) ;
#8659 = ORIENTED_EDGE ( 'NONE', *, *, #800, .F. ) ;
#8660 = FACE_OUTER_BOUND ( 'NONE', #5363, .T. ) ;
#8661 = AXIS2_PLACEMENT_3D ( 'NONE', #2958, #5374, #8292 ) ;
#8662 = ORIENTED_EDGE ( 'NONE', *, *, #1004, .T. ) ;
#8663 = DIRECTION ( 'NONE',  ( 0.000000000000000000, 0.000000000000000000, -1.000000000000000000 ) ) ;
#8664 = LINE ( 'NONE', #7171, #3011 ) ;
#8665 = DIRECTION ( 'NONE',  ( -1.000000000000000000, 0.000000000000000000, 0.000000000000000000 ) ) ;
#8666 = AXIS2_PLACEMENT_3D ( 'NONE', #9121, #247, #339 ) ;
#8667 = DIRECTION ( 'NONE',  ( 0.000000000000000000, 0.000000000000000000, -1.000000000000000000 ) ) ;
#8668 = CARTESIAN_POINT ( 'NONE',  ( 60.00000000000000000, 29.99999999999999645, -82.50000000000000000 ) ) ;
#8669 = ORIENTED_EDGE ( 'NONE', *, *, #950, .T. ) ;
#8670 = CIRCLE ( 'NONE', #9142, 3.000000000000002665 ) ;
#8671 = ORIENTED_EDGE ( 'NONE', *, *, #1735, .T. ) ;
#8672 = DIRECTION ( 'NONE',  ( -1.000000000000000000, -0.000000000000000000, -0.000000000000000000 ) ) ;
#8673 = ORIENTED_EDGE ( 'NONE', *, *, #6156, .F. ) ;
#8674 = CARTESIAN_POINT ( 'NONE',  ( 28.50000000000000355, 2.364097880450372804E-13, 1.500000000000041078 ) ) ;
#8675 = DIRECTION ( 'NONE',  ( -1.000000000000000000, -0.000000000000000000, -0.000000000000000000 ) ) ;
#8676 = CARTESIAN_POINT ( 'NONE',  ( 16.00000000000000000, 43.00000000000000000, -7.366666666666667140 ) ) ;
#8677 = DIRECTION ( 'NONE',  ( -1.000000000000000000, -0.000000000000000000, -0.000000000000000000 ) ) ;
#8678 = AXIS2_PLACEMENT_3D ( 'NONE', #7345, #3744, #3122 ) ;
#8679 = CARTESIAN_POINT ( 'NONE',  ( -26.99999999999998934, 35.00000000000000000, 5.000000000000004441 ) ) ;
#8680 = CARTESIAN_POINT ( 'NONE',  ( 0.000000000000000000, 22.50000000000000355, 5.000000000000000000 ) ) ;
#8681 = ORIENTED_EDGE ( 'NONE', *, *, #3957, .F. ) ;
#8682 = EDGE_LOOP ( 'NONE', ( #346, #6378, #6474, #9412 ) ) ;
#8683 = VECTOR ( 'NONE', #4468, 1000.000000000000000 ) ;
#8684 = CARTESIAN_POINT ( 'NONE',  ( 4.000000000000000000, -7.653668647303860872, -18.47759065022490432 ) ) ;
#8685 = LINE ( 'NONE', #2104, #3030 ) ;
#8686 = AXIS2_PLACEMENT_3D ( 'NONE', #8332, #7611, #1751 ) ;
#8687 = CIRCLE ( 'NONE', #6528, 7.250000000000002665 ) ;
#8688 = DIRECTION ( 'NONE',  ( 1.000000000000000000, 0.000000000000000000, 0.000000000000000000 ) ) ;
#8689 = FACE_OUTER_BOUND ( 'NONE', #9016, .T. ) ;
#8690 = VERTEX_POINT ( 'NONE', #4286 ) ;
#8691 = ORIENTED_EDGE ( 'NONE', *, *, #2008, .T. ) ;
#8692 = ORIENTED_EDGE ( 'NONE', *, *, #8651, .T. ) ;
#8693 = VECTOR ( 'NONE', #20, 1000.000000000000000 ) ;
#8694 = ORIENTED_EDGE ( 'NONE', *, *, #4314, .T. ) ;
#8695 = EDGE_CURVE ( 'NONE', #956, #5576, #3487, .T. ) ;
#8696 = CARTESIAN_POINT ( 'NONE',  ( 39.50000000000000000, 15.00000000000001066, -97.50000000000000000 ) ) ;
#8697 = ADVANCED_FACE ( 'NONE', ( #9370, #7111 ), #8512, .T. ) ;
#8698 = ADVANCED_FACE ( 'NONE', ( #1205 ), #4258, .T. ) ;
#8699 = DIRECTION ( 'NONE',  ( -0.000000000000000000, -0.000000000000000000, 1.000000000000000000 ) ) ;
#8700 = CIRCLE ( 'NONE', #3955, 18.49999999999997513 ) ;
#8701 = CARTESIAN_POINT ( 'NONE',  ( -2.999999999999842792, -22.50000000000000355, 5.000000000000000000 ) ) ;
#8702 = CIRCLE ( 'NONE', #4719, 30.00000000000000000 ) ;
#8703 = CARTESIAN_POINT ( 'NONE',  ( -26.21170834203229205, 53.97171801779368394, 11.99999999999999645 ) ) ;
#8704 = VECTOR ( 'NONE', #1015, 1000.000000000000000 ) ;
#8705 = CIRCLE ( 'NONE', #6113, 6.000000000000001776 ) ;
#8706 = DIRECTION ( 'NONE',  ( -0.7071067811865456854, -3.969829082701935600E-15, 0.7071067811865493491 ) ) ;
#8707 = VECTOR ( 'NONE', #1138, 1000.000000000000000 ) ;
#8708 = EDGE_LOOP ( 'NONE', ( #2838, #3208, #8662, #5286 ) ) ;
#8709 = CARTESIAN_POINT ( 'NONE',  ( 37.00000000000000000, -15.90990257669733943, -82.90990257669729147 ) ) ;
#8710 = ORIENTED_EDGE ( 'NONE', *, *, #2836, .F. ) ;
#8711 = AXIS2_PLACEMENT_3D ( 'NONE', #7095, #1867, #6300 ) ;
#8712 = CARTESIAN_POINT ( 'NONE',  ( 19.62310601229373574, -19.62310601229373574, 37.12563132923541787 ) ) ;
#8713 = DIRECTION ( 'NONE',  ( -1.000000000000000000, -0.000000000000000000, -0.000000000000000000 ) ) ;
#8714 = CIRCLE ( 'NONE', #6728, 8.000000000000021316 ) ;
#8715 = EDGE_CURVE ( 'NONE', #3397, #6362, #9267, .T. ) ;
#8716 = DIRECTION ( 'NONE',  ( 0.000000000000000000, 0.000000000000000000, 1.000000000000000000 ) ) ;
#8717 = MECHANICAL_DESIGN_GEOMETRIC_PRESENTATION_REPRESENTATION (  '', ( #6579 ), #1046 ) ;
#8718 = CARTESIAN_POINT ( 'NONE',  ( 51.96152422706632024, 29.99999999999999645, -12.99999999999999822 ) ) ;
#8719 = DIRECTION ( 'NONE',  ( -1.000000000000000000, 0.000000000000000000, 0.000000000000000000 ) ) ;
#8720 = ORIENTED_EDGE ( 'NONE', *, *, #6709, .T. ) ;
#8721 = ADVANCED_FACE ( 'NONE', ( #4906 ), #8602, .F. ) ;
#8722 = ORIENTED_EDGE ( 'NONE', *, *, #8363, .F. ) ;
#8723 = ORIENTED_EDGE ( 'NONE', *, *, #9381, .T. ) ;
#8724 = CARTESIAN_POINT ( 'NONE',  ( -28.14436749771988389, -2.074924133078855704, 1.218150816307263851 ) ) ;
#8725 = DIRECTION ( 'NONE',  ( 0.000000000000000000, 0.000000000000000000, -1.000000000000000000 ) ) ;
#8726 = AXIS2_PLACEMENT_3D ( 'NONE', #5163, #1461, #7226 ) ;
#8727 = DIRECTION ( 'NONE',  ( 1.000000000000000000, 0.000000000000000000, 0.000000000000000000 ) ) ;
#8728 = AXIS2_PLACEMENT_3D ( 'NONE', #8936, #6544, #5293 ) ;
#8729 = DIRECTION ( 'NONE',  ( 0.000000000000000000, 0.000000000000000000, -1.000000000000000000 ) ) ;
#8730 = DIRECTION ( 'NONE',  ( 0.000000000000000000, 0.000000000000000000, -1.000000000000000000 ) ) ;
#8731 = AXIS2_PLACEMENT_3D ( 'NONE', #2892, #1588, #6599 ) ;
#8732 = DIRECTION ( 'NONE',  ( 0.000000000000000000, 0.000000000000000000, 1.000000000000000000 ) ) ;
#8733 = ORIENTED_EDGE ( 'NONE', *, *, #5557, .F. ) ;
#8734 = ORIENTED_EDGE ( 'NONE', *, *, #3128, .T. ) ;
#8735 = CARTESIAN_POINT ( 'NONE',  ( 0.000000000000000000, 0.000000000000000000, 21.00000000000000000 ) ) ;
#8736 = CARTESIAN_POINT ( 'NONE',  ( 2.750000000000006661, 0.7500000000000000000, 0.000000000000000000 ) ) ;
#8737 = EDGE_CURVE ( 'NONE', #2697, #1434, #7024, .T. ) ;
#8738 = FACE_BOUND ( 'NONE', #9409, .T. ) ;
#8739 = DIRECTION ( 'NONE',  ( -1.000000000000000000, 0.000000000000000000, 0.000000000000000000 ) ) ;
#8740 = ORIENTED_EDGE ( 'NONE', *, *, #1095, .F. ) ;
#8741 = EDGE_CURVE ( 'NONE', #18, #7294, #279, .T. ) ;
#8742 = ORIENTED_EDGE ( 'NONE', *, *, #6250, .T. ) ;
#8743 = ORIENTED_EDGE ( 'NONE', *, *, #7933, .T. ) ;
#8744 = ORIENTED_EDGE ( 'NONE', *, *, #308, .F. ) ;
#8745 = LINE ( 'NONE', #57, #5777 ) ;
#8746 = CARTESIAN_POINT ( 'NONE',  ( -31.99999999999999289, 29.99999999999997868, 64.00000000000000000 ) ) ;
#8747 = CARTESIAN_POINT ( 'NONE',  ( -12.50000000000000000, 0.000000000000000000, 28.50000000000000355 ) ) ;
#8748 = LINE ( 'NONE', #3850, #7238 ) ;
#8749 = PLANE ( 'NONE',  #1680 ) ;
#8750 = CYLINDRICAL_SURFACE ( 'NONE', #5019, 3.000000000000000444 ) ;
#8751 = VECTOR ( 'NONE', #179, 1000.000000000000000 ) ;
#8752 = ORIENTED_EDGE ( 'NONE', *, *, #4026, .T. ) ;
#8753 = DIRECTION ( 'NONE',  ( -1.000000000000000000, 0.000000000000000000, 0.000000000000000000 ) ) ;
#8754 = VERTEX_POINT ( 'NONE', #7839 ) ;
#8755 = DIRECTION ( 'NONE',  ( -1.000000000000000000, 0.000000000000000000, -0.000000000000000000 ) ) ;
#8756 = CARTESIAN_POINT ( 'NONE',  ( 1.571166602479410136E-13, -22.50000000000000355, 10.00000000000000000 ) ) ;
#8757 = EDGE_CURVE ( 'NONE', #6239, #4910, #3509, .T. ) ;
#8758 = AXIS2_PLACEMENT_3D ( 'NONE', #2133, #4197, #2808 ) ;
#8760 = ADVANCED_FACE ( 'NONE', ( #8469 ), #570, .T. ) ;
#8759 = FACE_OUTER_BOUND ( 'NONE', #1845, .T. ) ;
#8761 = FACE_OUTER_BOUND ( 'NONE', #242, .T. ) ;
#8762 = CARTESIAN_POINT ( 'NONE',  ( -30.00000000000000000, 3.673940397442059178E-15, 3.000000000000052847 ) ) ;
#8763 = PRODUCT_DEFINITION_SHAPE ( 'NONE', 'NONE',  #9490 ) ;
#8764 = ORIENTED_EDGE ( 'NONE', *, *, #3370, .T. ) ;
#8765 = ORIENTED_EDGE ( 'NONE', *, *, #1111, .T. ) ;
#8766 = DIRECTION ( 'NONE',  ( 1.000000000000000000, 0.000000000000000000, 0.000000000000000000 ) ) ;
#8767 = VERTEX_POINT ( 'NONE', #5687 ) ;
#8768 = DIRECTION ( 'NONE',  ( 1.000000000000000000, 0.000000000000000000, 0.000000000000000000 ) ) ;
#8769 = DIRECTION ( 'NONE',  ( -1.000000000000000000, 0.000000000000000000, 0.000000000000000000 ) ) ;
#8770 = FACE_OUTER_BOUND ( 'NONE', #626, .T. ) ;
#8771 = AXIS2_PLACEMENT_3D ( 'NONE', #677, #2847, #8515 ) ;
#8772 = CARTESIAN_POINT ( 'NONE',  ( -3.000000000000000000, -22.50000000000000355, 5.000000000000000000 ) ) ;
#8773 = FACE_OUTER_BOUND ( 'NONE', #3479, .T. ) ;
#8774 = DIRECTION ( 'NONE',  ( 3.969829082701938755E-15, -0.7071067811865493491, -0.7071067811865455743 ) ) ;
#8775 = CARTESIAN_POINT ( 'NONE',  ( 2.143131898507868248E-15, -17.50000000000000000, 14.49999999999999822 ) ) ;
#8776 = ORIENTED_EDGE ( 'NONE', *, *, #5637, .T. ) ;
#8777 = ORIENTED_EDGE ( 'NONE', *, *, #1720, .T. ) ;
#8778 = DIRECTION ( 'NONE',  ( -1.000000000000000000, 0.000000000000000000, 0.000000000000000000 ) ) ;
#8779 = CARTESIAN_POINT ( 'NONE',  ( 17.50000000000000355, 0.000000000000000000, 49.50000000000000000 ) ) ;
#8780 = CIRCLE ( 'NONE', #3562, 3.000000000000000000 ) ;
#8781 = DIRECTION ( 'NONE',  ( 1.000000000000000000, 0.000000000000000000, 0.000000000000000000 ) ) ;
#8782 = CARTESIAN_POINT ( 'NONE',  ( 4.000000000000000000, -18.47759065022712832, 6.903668647304566974 ) ) ;
#8783 = VERTEX_POINT ( 'NONE', #2026 ) ;
#8784 = VERTEX_POINT ( 'NONE', #2071 ) ;
#8785 = CIRCLE ( 'NONE', #4653, 0.7500000000017874591 ) ;
#8786 = ORIENTED_EDGE ( 'NONE', *, *, #1031, .T. ) ;
#8787 = DIRECTION ( 'NONE',  ( 0.9940155806428060403, 0.002596178474115097209, 0.1092075331498506829 ) ) ;
#8788 = ORIENTED_EDGE ( 'NONE', *, *, #8413, .F. ) ;
#8789 = DIRECTION ( 'NONE',  ( -1.000000000000000000, 0.000000000000000000, 0.000000000000000000 ) ) ;
#8790 = LINE ( 'NONE', #768, #7934 ) ;
#8791 = CYLINDRICAL_SURFACE ( 'NONE', #4276, 1.560000000001466436 ) ;
#8792 = DIRECTION ( 'NONE',  ( -1.000000000000000000, 0.000000000000000000, 0.000000000000000000 ) ) ;
#8793 = FACE_OUTER_BOUND ( 'NONE', #5502, .T. ) ;
#8794 = LINE ( 'NONE', #5198, #2571 ) ;
#8795 = VERTEX_POINT ( 'NONE', #7929 ) ;
#8796 = CARTESIAN_POINT ( 'NONE',  ( 18.49999999999997513, 0.000000000000000000, 64.00000000000000000 ) ) ;
#8797 = VERTEX_POINT ( 'NONE', #6315 ) ;
#8798 = CARTESIAN_POINT ( 'NONE',  ( 0.000000000000000000, 0.000000000000000000, 27.50000000000000355 ) ) ;
#8799 = LINE ( 'NONE', #5979, #1789 ) ;
#8800 = CARTESIAN_POINT ( 'NONE',  ( -53.29490495164537833, -3.673940397442057600E-15, -70.00000000000000000 ) ) ;
#8801 = AXIS2_PLACEMENT_3D ( 'NONE', #3933, #6965, #6157 ) ;
#8802 = CARTESIAN_POINT ( 'NONE',  ( 0.000000000000000000, 0.000000000000000000, 0.000000000000000000 ) ) ;
#8803 = CIRCLE ( 'NONE', #8039, 6.000000000000000000 ) ;
#8804 = ORIENTED_EDGE ( 'NONE', *, *, #3370, .F. ) ;
#8805 = ORIENTED_EDGE ( 'NONE', *, *, #1121, .T. ) ;
#8806 = CARTESIAN_POINT ( 'NONE',  ( 53.29490495164537833, -27.56180520566615044, -81.40266088840111536 ) ) ;
#8807 = ORIENTED_EDGE ( 'NONE', *, *, #1848, .F. ) ;
#8808 = CARTESIAN_POINT ( 'NONE',  ( 0.000000000000000000, 34.00000000000001421, 49.50000000000000000 ) ) ;
#8809 = EDGE_CURVE ( 'NONE', #7685, #2348, #4108, .T. ) ;
#8810 = VECTOR ( 'NONE', #8774, 1000.000000000000114 ) ;
#8811 = PLANE ( 'NONE',  #4740 ) ;
#8812 = FACE_OUTER_BOUND ( 'NONE', #5490, .T. ) ;
#8813 = EDGE_CURVE ( 'NONE', #4316, #6932, #1883, .T. ) ;
#8814 = VECTOR ( 'NONE', #1238, 1000.000000000000000 ) ;
#8815 = EDGE_CURVE ( 'NONE', #6613, #6513, #7254, .T. ) ;
#8816 = EDGE_CURVE ( 'NONE', #386, #5908, #8705, .T. ) ;
#8817 = CYLINDRICAL_SURFACE ( 'NONE', #3380, 3.000000000000002665 ) ;
#8818 = DIRECTION ( 'NONE',  ( -1.000000000000000000, -0.000000000000000000, -0.000000000000000000 ) ) ;
#8819 = CARTESIAN_POINT ( 'NONE',  ( -31.99999999999999289, -29.99999999999996447, 64.00000000000000000 ) ) ;
#8820 = CYLINDRICAL_SURFACE ( 'NONE', #1339, 6.000000000000000888 ) ;
#8821 = EDGE_LOOP ( 'NONE', ( #3881, #2667, #4835, #8144 ) ) ;
#8822 = ORIENTED_EDGE ( 'NONE', *, *, #3400, .T. ) ;
#8823 = CARTESIAN_POINT ( 'NONE',  ( 0.000000000000000000, 35.00000000000000000, 32.00000000000000000 ) ) ;
#8824 = ORIENTED_EDGE ( 'NONE', *, *, #6195, .T. ) ;
#8825 = AXIS2_PLACEMENT_3D ( 'NONE', #8168, #199, #5862 ) ;
#8826 = CARTESIAN_POINT ( 'NONE',  ( 6.193323906411744240, 26.79012200670185351, 0.4900784328797758715 ) ) ;
#8827 = EDGE_CURVE ( 'NONE', #1163, #7881, #99, .T. ) ;
#8828 = DIRECTION ( 'NONE',  ( 0.000000000000000000, -0.000000000000000000, 1.000000000000000000 ) ) ;
#8829 = CARTESIAN_POINT ( 'NONE',  ( -57.72192878071319910, -19.00148731544556568, -33.94573509506513176 ) ) ;
#8830 = AXIS2_PLACEMENT_3D ( 'NONE', #8214, #8977, #8494 ) ;
#8831 = ORIENTED_EDGE ( 'NONE', *, *, #5962, .F. ) ;
#8832 = ORIENTED_EDGE ( 'NONE', *, *, #7232, .F. ) ;
#8833 = EDGE_CURVE ( 'NONE', #7481, #152, #2735, .T. ) ;
#8834 = ORIENTED_EDGE ( 'NONE', *, *, #5117, .T. ) ;
#8835 = DIRECTION ( 'NONE',  ( 0.7071067811865456854, 0.7071067811865493491, -0.000000000000000000 ) ) ;
#8836 = CARTESIAN_POINT ( 'NONE',  ( 19.74999999999999645, 43.00000000000000000, -25.00000000000000000 ) ) ;
#8837 = CIRCLE ( 'NONE', #100, 1.560000000002236709 ) ;
#8838 = LINE ( 'NONE', #4376, #2896 ) ;
#8839 = DIRECTION ( 'NONE',  ( -1.000000000000000000, -0.000000000000000000, -0.000000000000000000 ) ) ;
#8840 = DIRECTION ( 'NONE',  ( 0.000000000000000000, 0.000000000000000000, 1.000000000000000000 ) ) ;
#8841 = DIRECTION ( 'NONE',  ( -1.000000000000000000, 0.000000000000000000, 0.000000000000000000 ) ) ;
#8842 = ORIENTED_EDGE ( 'NONE', *, *, #4128, .F. ) ;
#8843 = CONICAL_SURFACE ( 'NONE', #5482, 17.50000000000000355, 0.7853981633974466137 ) ;
#8844 = CARTESIAN_POINT ( 'NONE',  ( 0.000000000000000000, -14.14213562373248401, -12.58213562372718641 ) ) ;
#8845 = VERTEX_POINT ( 'NONE', #2163 ) ;
#8846 =( REPRESENTATION_RELATIONSHIP ('NONE','NONE', #1933, #8501 ) REPRESENTATION_RELATIONSHIP_WITH_TRANSFORMATION ( #6343 )SHAPE_REPRESENTATION_RELATIONSHIP( ) );
#8847 = DIRECTION ( 'NONE',  ( -0.000000000000000000, -0.000000000000000000, -1.000000000000000000 ) ) ;
#8848 = FACE_OUTER_BOUND ( 'NONE', #5585, .T. ) ;
#8849 = VECTOR ( 'NONE', #2837, 1000.000000000000114 ) ;
#8850 = VECTOR ( 'NONE', #6442, 1000.000000000000114 ) ;
#8851 = CARTESIAN_POINT ( 'NONE',  ( -19.74999999999999645, -43.00000000000000000, 11.99999999999999645 ) ) ;
#8852 = EDGE_CURVE ( 'NONE', #4140, #4695, #6542, .T. ) ;
#8853 = CIRCLE ( 'NONE', #7324, 17.50000000000000355 ) ;
#8854 = CYLINDRICAL_SURFACE ( 'NONE', #6478, 15.00000000000000000 ) ;
#8855 = VECTOR ( 'NONE', #4549, 1000.000000000000114 ) ;
#8856 = EDGE_LOOP ( 'NONE', ( #6085, #3912, #4326, #7046 ) ) ;
#8857 = VECTOR ( 'NONE', #3118, 1000.000000000000000 ) ;
#8858 = ADVANCED_FACE ( 'NONE', ( #4331 ), #7981, .F. ) ;
#8859 = VERTEX_POINT ( 'NONE', #4375 ) ;
#8860 = CARTESIAN_POINT ( 'NONE',  ( 0.4129292217237342522, 28.50085334706577100, 1.500673695285823506 ) ) ;
#8861 = AXIS2_PLACEMENT_3D ( 'NONE', #8735, #5898, #8778 ) ;
#8862 = EDGE_LOOP ( 'NONE', ( #4552, #5338, #5622, #1631 ) ) ;
#8863 = DIRECTION ( 'NONE',  ( 0.000000000000000000, 0.000000000000000000, 1.000000000000000000 ) ) ;
#8864 = FACE_OUTER_BOUND ( 'NONE', #9310, .T. ) ;
#8865 = DIRECTION ( 'NONE',  ( -0.000000000000000000, -0.000000000000000000, 1.000000000000000000 ) ) ;
#8866 = VECTOR ( 'NONE', #327, 1000.000000000000000 ) ;
#8867 = LINE ( 'NONE', #40, #7985 ) ;
#8868 = CARTESIAN_POINT ( 'NONE',  ( 0.7500000000000000000, -2.750000000000002665, 1.500000000000000000 ) ) ;
#8869 = CARTESIAN_POINT ( 'NONE',  ( -0.7500000000000000000, -0.7500000000000000000, 1.500000000000000000 ) ) ;
#8870 = DIRECTION ( 'NONE',  ( 0.000000000000000000, 0.000000000000000000, -1.000000000000000000 ) ) ;
#8871 = ORIENTED_EDGE ( 'NONE', *, *, #7669, .F. ) ;
#8872 = ORIENTED_EDGE ( 'NONE', *, *, #2766, .F. ) ;
#8873 = CIRCLE ( 'NONE', #5508, 3.000000000000002665 ) ;
#8874 = CARTESIAN_POINT ( 'NONE',  ( -15.99999999999999645, -49.08300322764475254, -4.730698601353939381 ) ) ;
#8875 = AXIS2_PLACEMENT_3D ( 'NONE', #445, #6456, #4095 ) ;
#8876 = ORIENTED_EDGE ( 'NONE', *, *, #1615, .F. ) ;
#8877 = CARTESIAN_POINT ( 'NONE',  ( 0.000000000000000000, -18.47759065022712832, 7.653668647304757044 ) ) ;
#8878 = AXIS2_PLACEMENT_3D ( 'NONE', #1369, #4490, #7417 ) ;
#8879 = ADVANCED_FACE ( 'NONE', ( #6638 ), #9158, .F. ) ;
#8880 = AXIS2_PLACEMENT_3D ( 'NONE', #3470, #5603, #5746 ) ;
#8881 = FACE_OUTER_BOUND ( 'NONE', #3226, .T. ) ;
#8882 = CARTESIAN_POINT ( 'NONE',  ( -60.00000000000001421, -9.637301612213116542, -29.99999999999998934 ) ) ;
#8883 = ORIENTED_EDGE ( 'NONE', *, *, #5348, .T. ) ;
#8884 = VERTEX_POINT ( 'NONE', #3748 ) ;
#8885 = SHAPE_DEFINITION_REPRESENTATION ( #5929, #1933 ) ;
#8886 = CARTESIAN_POINT ( 'NONE',  ( -37.00000000000000711, 15.90990257669733943, -85.90990257669729147 ) ) ;
#8887 = DIRECTION ( 'NONE',  ( -1.000000000000000000, 0.000000000000000000, 0.000000000000000000 ) ) ;
#8888 = DIRECTION ( 'NONE',  ( 0.000000000000000000, 0.000000000000000000, -1.000000000000000000 ) ) ;
#8889 = DIRECTION ( 'NONE',  ( 0.000000000000000000, 0.000000000000000000, -1.000000000000000000 ) ) ;
#8890 = DIRECTION ( 'NONE',  ( 1.000000000000000000, 0.000000000000000000, 0.000000000000000000 ) ) ;
#8891 = DIRECTION ( 'NONE',  ( 0.000000000000000000, 1.000000000000000000, 0.000000000000000000 ) ) ;
#8892 = AXIS2_PLACEMENT_3D ( 'NONE', #5778, #7029, #1206 ) ;
#8893 = ORIENTED_EDGE ( 'NONE', *, *, #2143, .T. ) ;
#8894 = ORIENTED_EDGE ( 'NONE', *, *, #7281, .F. ) ;
#8895 = LINE ( 'NONE', #2854, #4795 ) ;
#8896 = DIRECTION ( 'NONE',  ( 0.000000000000000000, 0.000000000000000000, 1.000000000000000000 ) ) ;
#8897 = DIRECTION ( 'NONE',  ( 0.000000000000000000, 0.7071067811865426878, 0.7071067811865524577 ) ) ;
#8898 = LINE ( 'NONE', #3718, #2332 ) ;
#8899 = AXIS2_PLACEMENT_3D ( 'NONE', #4753, #288, #1088 ) ;
#8900 = ORIENTED_EDGE ( 'NONE', *, *, #8411, .F. ) ;
#8901 = ORIENTED_EDGE ( 'NONE', *, *, #8520, .T. ) ;
#8902 = ORIENTED_EDGE ( 'NONE', *, *, #7618, .F. ) ;
#8903 = CARTESIAN_POINT ( 'NONE',  ( -0.2247925377428787452, 28.49955466461979015, 1.499648419317238357 ) ) ;
#8904 = EDGE_LOOP ( 'NONE', ( #5403, #6147, #1117, #4770 ) ) ;
#8905 = DIRECTION ( 'NONE',  ( 0.000000000000000000, 0.000000000000000000, 1.000000000000000000 ) ) ;
#8906 = DIRECTION ( 'NONE',  ( 0.000000000000000000, 1.000000000000000000, 0.000000000000000000 ) ) ;
#8907 = VECTOR ( 'NONE', #4918, 1000.000000000000000 ) ;
#8908 = CARTESIAN_POINT ( 'NONE',  ( 0.000000000000000000, -22.50000000000000355, 10.00000000000000000 ) ) ;
#8909 = EDGE_CURVE ( 'NONE', #8784, #3755, #8790, .T. ) ;
#8910 = DIRECTION ( 'NONE',  ( 0.7071067811865426878, 8.659560562354874926E-17, -0.7071067811865524577 ) ) ;
#8911 = EDGE_CURVE ( 'NONE', #2503, #3864, #1965, .T. ) ;
#8912 = LINE ( 'NONE', #7421, #9257 ) ;
#8913 = CARTESIAN_POINT ( 'NONE',  ( 5.000000000000000000, -18.47759065022712832, 7.653668647304757044 ) ) ;
#8914 = DIRECTION ( 'NONE',  ( -1.000000000000000000, -0.000000000000000000, -0.000000000000000000 ) ) ;
#8915 = ORIENTED_EDGE ( 'NONE', *, *, #22, .T. ) ;
#8916 = ORIENTED_EDGE ( 'NONE', *, *, #441, .T. ) ;
#8917 =( BOUNDED_CURVE ( )  B_SPLINE_CURVE ( 3, ( #5177, #4408, #1676, #8779 ),
 .UNSPECIFIED., .F., .T. ) 
 B_SPLINE_CURVE_WITH_KNOTS ( ( 4, 4 ),
 ( 5.497787143782137953, 6.283185307179586232 ),
 .UNSPECIFIED. ) 
 CURVE ( )  GEOMETRIC_REPRESENTATION_ITEM ( )  RATIONAL_B_SPLINE_CURVE ( ( 1.000000000000000000, 0.9492530216741911220, 0.9492530216741911220, 1.000000000000000000 ) ) 
 REPRESENTATION_ITEM ( '' )  );
#8918 = DIRECTION ( 'NONE',  ( 0.000000000000000000, 0.000000000000000000, 1.000000000000000000 ) ) ;
#8919 = ORIENTED_EDGE ( 'NONE', *, *, #1418, .F. ) ;
#8920 = AXIS2_PLACEMENT_3D ( 'NONE', #5462, #8667, #8576 ) ;
#8921 = PRODUCT_DEFINITION_SHAPE ( 'NONE', 'NONE',  #9486 ) ;
#8922 = EDGE_CURVE ( 'NONE', #8859, #2372, #3583, .T. ) ;
#8923 = LINE ( 'NONE', #49, #9472 ) ;
#8924 = DIRECTION ( 'NONE',  ( -0.000000000000000000, -0.000000000000000000, -1.000000000000000000 ) ) ;
#8925 = PRODUCT_DEFINITION_CONTEXT ( 'detailed design', #203, 'design' ) ;
#8926 = FACE_OUTER_BOUND ( 'NONE', #6097, .T. ) ;
#8927 = ORIENTED_EDGE ( 'NONE', *, *, #5865, .F. ) ;
#8928 = ORIENTED_EDGE ( 'NONE', *, *, #5557, .T. ) ;
#8929 = DIRECTION ( 'NONE',  ( 5.637851296924809487E-18, -0.9997175446104182850, 0.02376617340079525617 ) ) ;
#8930 = EDGE_CURVE ( 'NONE', #6850, #1286, #8853, .T. ) ;
#8931 = DIRECTION ( 'NONE',  ( -0.000000000000000000, -0.000000000000000000, -1.000000000000000000 ) ) ;
#8932 = DIRECTION ( 'NONE',  ( -1.000000000000000000, 0.000000000000000000, 0.000000000000000000 ) ) ;
#8933 = ADVANCED_FACE ( 'NONE', ( #1440 ), #2889, .F. ) ;
#8934 = EDGE_CURVE ( 'NONE', #9435, #6389, #11, .T. ) ;
#8935 = EDGE_CURVE ( 'NONE', #9218, #8795, #6268, .T. ) ;
#8936 = CARTESIAN_POINT ( 'NONE',  ( 0.000000000000000000, 0.000000000000000000, 3.000000000000052847 ) ) ;
#8937 = CARTESIAN_POINT ( 'NONE',  ( -28.50000000000000355, 0.000000000000000000, 2.000000000000039080 ) ) ;
#8938 = CIRCLE ( 'NONE', #7098, 6.000000000000001776 ) ;
#8939 = CARTESIAN_POINT ( 'NONE',  ( -22.50000000000000000, -7.855833012397050680E-14, 5.000000000000000000 ) ) ;
#8940 = DIRECTION ( 'NONE',  ( -0.000000000000000000, -0.000000000000000000, -1.000000000000000000 ) ) ;
#8941 = LINE ( 'NONE', #8762, #6501 ) ;
#8942 = ORIENTED_EDGE ( 'NONE', *, *, #15, .T. ) ;
#8943 = DIRECTION ( 'NONE',  ( 1.000000000000000000, 0.000000000000000000, 0.000000000000000000 ) ) ;
#8944 = VERTEX_POINT ( 'NONE', #3659 ) ;
#8945 = CARTESIAN_POINT ( 'NONE',  ( -12.50000000000000000, 0.000000000000000000, 48.00000000000036948 ) ) ;
#8946 = DIRECTION ( 'NONE',  ( 0.000000000000000000, 0.000000000000000000, -1.000000000000000000 ) ) ;
#8947 = EDGE_CURVE ( 'NONE', #8797, #8189, #6596, .T. ) ;
#8948 = AXIS2_PLACEMENT_3D ( 'NONE', #1172, #6233, #3342 ) ;
#8949 = EDGE_CURVE ( 'NONE', #9261, #5549, #5943, .T. ) ;
#8950 = CARTESIAN_POINT ( 'NONE',  ( 4.000000000000000000, 7.653668647302530381, 18.47759065022802716 ) ) ;
#8951 = CARTESIAN_POINT ( 'NONE',  ( -53.29490495164537833, -15.90990257669733943, -88.90990257669730568 ) ) ;
#8952 = EDGE_CURVE ( 'NONE', #9262, #3397, #4514, .T. ) ;
#8953 = VERTEX_POINT ( 'NONE', #860 ) ;
#8954 = ORIENTED_EDGE ( 'NONE', *, *, #8935, .T. ) ;
#8955 = EDGE_LOOP ( 'NONE', ( #7488, #1570, #2358, #5597 ) ) ;
#8956 = ORIENTED_EDGE ( 'NONE', *, *, #9357, .F. ) ;
#8957 = FACE_OUTER_BOUND ( 'NONE', #8433, .T. ) ;
#8958 = CARTESIAN_POINT ( 'NONE',  ( 6.000000000000000888, 22.50000000000000355, 2.000000000000013767 ) ) ;
#8959 = CONICAL_SURFACE ( 'NONE', #3134, 30.00000000000000000, 0.7853981633974488341 ) ;
#8960 = CARTESIAN_POINT ( 'NONE',  ( -37.22467645238198486, -47.05659850664388699, -0.5000000000000038858 ) ) ;
#8961 = DIRECTION ( 'NONE',  ( 0.000000000000000000, 0.000000000000000000, -1.000000000000000000 ) ) ;
#8962 = CARTESIAN_POINT ( 'NONE',  ( 26.02777777777776436, -7.180166011355007427, 0.000000000000000000 ) ) ;
#8963 = ORIENTED_EDGE ( 'NONE', *, *, #8737, .F. ) ;
#8964 = AXIS2_PLACEMENT_3D ( 'NONE', #3920, #6092, #1616 ) ;
#8965 = ORIENTED_EDGE ( 'NONE', *, *, #2328, .F. ) ;
#8966 = DIRECTION ( 'NONE',  ( -0.000000000000000000, -0.000000000000000000, -1.000000000000000000 ) ) ;
#8967 = ORIENTED_EDGE ( 'NONE', *, *, #7589, .F. ) ;
#8968 = FACE_BOUND ( 'NONE', #5, .T. ) ;
#8969 = AXIS2_PLACEMENT_3D ( 'NONE', #5319, #3918, #82 ) ;
#8970 = ORIENTED_EDGE ( 'NONE', *, *, #3140, .F. ) ;
#8971 = CARTESIAN_POINT ( 'NONE',  ( 12.55753963192706557, 30.00000000000000000, -8.879521428754532764 ) ) ;
#8972 = CARTESIAN_POINT ( 'NONE',  ( 51.96152422706632734, -30.00000000000000000, -80.85015119857384036 ) ) ;
#8973 = CARTESIAN_POINT ( 'NONE',  ( 27.00000000000000355, -29.99999999999999289, 64.00000000000000000 ) ) ;
#8974 = ORIENTED_EDGE ( 'NONE', *, *, #6218, .F. ) ;
#8975 = ORIENTED_EDGE ( 'NONE', *, *, #3931, .T. ) ;
#8976 = VECTOR ( 'NONE', #7048, 1000.000000000000000 ) ;
#8977 = DIRECTION ( 'NONE',  ( -1.000000000000000000, 0.000000000000000000, 0.000000000000000000 ) ) ;
#8978 = LINE ( 'NONE', #5345, #3645 ) ;
#8979 = DIRECTION ( 'NONE',  ( -1.000000000000000000, 0.000000000000000000, 0.000000000000000000 ) ) ;
#8980 = PRODUCT_DEFINITION_FORMATION_WITH_SPECIFIED_SOURCE ( 'ANY', '', #5082, .NOT_KNOWN. ) ;
#8981 = FACE_OUTER_BOUND ( 'NONE', #4508, .T. ) ;
#8982 = CARTESIAN_POINT ( 'NONE',  ( -28.68405123480335916, 1.339801352072197860, 1.707604365230749766 ) ) ;
#8983 = VERTEX_POINT ( 'NONE', #8410 ) ;
#8984 = EDGE_CURVE ( 'NONE', #933, #3742, #9314, .T. ) ;
#8985 = DIRECTION ( 'NONE',  ( -0.000000000000000000, -0.000000000000000000, 1.000000000000000000 ) ) ;
#8986 = EDGE_CURVE ( 'NONE', #2437, #7251, #5436, .T. ) ;
#8987 = VERTEX_POINT ( 'NONE', #1732 ) ;
#8988 = AXIS2_PLACEMENT_3D ( 'NONE', #7862, #4166, #2090 ) ;
#8989 = DIRECTION ( 'NONE',  ( -0.000000000000000000, 1.000000000000000000, 0.000000000000000000 ) ) ;
#8990 = CYLINDRICAL_SURFACE ( 'NONE', #9150, 1.560000000000134168 ) ;
#8991 = FACE_BOUND ( 'NONE', #3404, .T. ) ;
#8992 = CARTESIAN_POINT ( 'NONE',  ( 6.000000000000000888, 22.50000000000000355, 5.000000000000000000 ) ) ;
#8993 = EDGE_CURVE ( 'NONE', #2280, #8784, #6163, .T. ) ;
#8994 = AXIS2_PLACEMENT_3D ( 'NONE', #837, #2340, #1664 ) ;
#8995 = MECHANICAL_DESIGN_GEOMETRIC_PRESENTATION_REPRESENTATION (  '', ( #6078 ), #2391 ) ;
#8996 = EDGE_LOOP ( 'NONE', ( #732, #2872, #4226, #2521 ) ) ;
#8997 = ORIENTED_EDGE ( 'NONE', *, *, #608, .T. ) ;
#8998 = VERTEX_POINT ( 'NONE', #5290 ) ;
#8999 = ORIENTED_EDGE ( 'NONE', *, *, #258, .F. ) ;
#9000 = DIRECTION ( 'NONE',  ( 0.000000000000000000, 0.000000000000000000, 1.000000000000000000 ) ) ;
#9001 = CARTESIAN_POINT ( 'NONE',  ( 27.00000000000000355, 29.99999999999997158, 0.000000000000000000 ) ) ;
#9002 = AXIS2_PLACEMENT_3D ( 'NONE', #682, #6604, #7987 ) ;
#9003 = DIRECTION ( 'NONE',  ( -1.000000000000000000, 0.000000000000000000, 0.000000000000000000 ) ) ;
#9004 = CIRCLE ( 'NONE', #7157, 0.7500000000013684609 ) ;
#9005 = DIRECTION ( 'NONE',  ( -1.000000000000000000, 0.000000000000000000, 0.000000000000000000 ) ) ;
#9006 = AXIS2_PLACEMENT_3D ( 'NONE', #5781, #8606, #5005 ) ;
#9007 = CARTESIAN_POINT ( 'NONE',  ( -28.00000000000000711, 0.000000000000000000, 10.00000000000000000 ) ) ;
#9008 = AXIS2_PLACEMENT_3D ( 'NONE', #8595, #4278, #7018 ) ;
#9009 = CARTESIAN_POINT ( 'NONE',  ( -29.49999999999999289, -29.99999999999997868, 61.49999999999998579 ) ) ;
#9010 = CIRCLE ( 'NONE', #1652, 22.50000000000000000 ) ;
#9011 = CARTESIAN_POINT ( 'NONE',  ( 27.28672223502584160, -5.374373886926188781, 0.8093214368023355920 ) ) ;
#9012 = AXIS2_PLACEMENT_3D ( 'NONE', #5192, #2977, #2118 ) ;
#9013 = ORIENTED_EDGE ( 'NONE', *, *, #844, .T. ) ;
#9014 = ORIENTED_EDGE ( 'NONE', *, *, #3726, .T. ) ;
#9015 = DIRECTION ( 'NONE',  ( -1.000000000000000000, -0.000000000000000000, -0.000000000000000000 ) ) ;
#9016 = EDGE_LOOP ( 'NONE', ( #4190, #1670, #1996, #4961 ) ) ;
#9017 = CIRCLE ( 'NONE', #1655, 3.000000000000002665 ) ;
#9018 = DIRECTION ( 'NONE',  ( -0.000000000000000000, -0.000000000000000000, -1.000000000000000000 ) ) ;
#9019 = EDGE_LOOP ( 'NONE', ( #856, #7604, #8632, #174 ) ) ;
#9020 = CARTESIAN_POINT ( 'NONE',  ( 19.50000000000000355, 0.000000000000000000, 5.000000000000000000 ) ) ;
#9021 = AXIS2_PLACEMENT_3D ( 'NONE', #1908, #6429, #9346 ) ;
#9022 = CARTESIAN_POINT ( 'NONE',  ( 60.00000000000000000, 15.90990257669733943, -51.09009742330271564 ) ) ;
#9023 = CARTESIAN_POINT ( 'NONE',  ( 7.180166011355011868, -26.02777777777776436, 0.000000000000000000 ) ) ;
#9024 = ORIENTED_EDGE ( 'NONE', *, *, #9403, .F. ) ;
#9025 = ORIENTED_EDGE ( 'NONE', *, *, #154, .T. ) ;
#9026 = EDGE_CURVE ( 'NONE', #8783, #2826, #1826, .T. ) ;
#9027 = CARTESIAN_POINT ( 'NONE',  ( 26.91620486903881115, -4.078357040894570851, 0.2218373908656700588 ) ) ;
#9028 = AXIS2_PLACEMENT_3D ( 'NONE', #2636, #4204, #3529 ) ;
#9029 = DIRECTION ( 'NONE',  ( -0.000000000000000000, -1.000000000000000000, -0.000000000000000000 ) ) ;
#9030 = CIRCLE ( 'NONE', #2754, 0.7499999999982936982 ) ;
#9031 =( REPRESENTATION_RELATIONSHIP ('NONE','NONE', #1933, #1625 ) REPRESENTATION_RELATIONSHIP_WITH_TRANSFORMATION ( #3938 )SHAPE_REPRESENTATION_RELATIONSHIP( ) );
#9032 = CARTESIAN_POINT ( 'NONE',  ( 0.000000000000000000, 2.694222958124177598E-15, 22.00000000000000711 ) ) ;
#9033 = EDGE_CURVE ( 'NONE', #472, #1938, #7690, .T. ) ;
#9034 = CYLINDRICAL_SURFACE ( 'NONE', #1963, 0.7500000000017874591 ) ;
#9035 = CARTESIAN_POINT ( 'NONE',  ( -12.37436867076458036, 12.37436867076458036, 44.37436867076458213 ) ) ;
#9036 = VECTOR ( 'NONE', #3800, 1000.000000000000000 ) ;
#9037 = VERTEX_POINT ( 'NONE', #246 ) ;
#9038 = SURFACE_SIDE_STYLE ('',( #968 ) ) ;
#9039 = ORIENTED_EDGE ( 'NONE', *, *, #2300, .T. ) ;
#9040 = LINE ( 'NONE', #5399, #2181 ) ;
#9041 = DIRECTION ( 'NONE',  ( 0.000000000000000000, 0.000000000000000000, 1.000000000000000000 ) ) ;
#9042 = CARTESIAN_POINT ( 'NONE',  ( 12.37436867076458036, 12.37436867076458036, 19.62563132923542142 ) ) ;
#9043 = DIRECTION ( 'NONE',  ( -0.000000000000000000, -0.000000000000000000, -1.000000000000000000 ) ) ;
#9044 = ORIENTED_EDGE ( 'NONE', *, *, #8052, .T. ) ;
#9045 = ORIENTED_EDGE ( 'NONE', *, *, #535, .T. ) ;
#9046 = ORIENTED_EDGE ( 'NONE', *, *, #8520, .F. ) ;
#9047 = ORIENTED_EDGE ( 'NONE', *, *, #7107, .T. ) ;
#9048 = PRODUCT_DEFINITION ( 'UNKNOWN', '', #2695, #7495 ) ;
#9049 = CARTESIAN_POINT ( 'NONE',  ( 60.00000000000000000, -15.90990257669733943, -54.09009742330271564 ) ) ;
#9050 = ADVANCED_FACE ( 'NONE', ( #4666 ), #1688, .F. ) ;
#9051 = DIRECTION ( 'NONE',  ( 0.000000000000000000, -1.000000000000000000, 0.000000000000000000 ) ) ;
#9052 = EDGE_CURVE ( 'NONE', #7912, #4290, #2616, .T. ) ;
#9053 = CARTESIAN_POINT ( 'NONE',  ( 0.000000000000000000, 22.50000000000000355, 5.000000000000000000 ) ) ;
#9054 = ADVANCED_FACE ( 'NONE', ( #3265 ), #4711, .F. ) ;
#9055 = CARTESIAN_POINT ( 'NONE',  ( 39.50000000000000000, -30.00000000000000355, -82.50000000000001421 ) ) ;
#9056 = EDGE_CURVE ( 'NONE', #4256, #804, #6601, .T. ) ;
#9057 = DIRECTION ( 'NONE',  ( -1.000000000000000000, 0.000000000000000000, -0.000000000000000000 ) ) ;
#9058 = CARTESIAN_POINT ( 'NONE',  ( 27.86926932341927809, -4.210987672173456708, 1.183815993626684104 ) ) ;
#9059 = ORIENTED_EDGE ( 'NONE', *, *, #4943, .F. ) ;
#9060 = ORIENTED_EDGE ( 'NONE', *, *, #5714, .T. ) ;
#9061 = DIRECTION ( 'NONE',  ( -0.8660254037844399289, 0.000000000000000000, -0.4999999999999977240 ) ) ;
#9062 = CIRCLE ( 'NONE', #4917, 18.50000000000000355 ) ;
#9063 = ORIENTED_EDGE ( 'NONE', *, *, #6043, .T. ) ;
#9064 = DIRECTION ( 'NONE',  ( -0.000000000000000000, -0.000000000000000000, -1.000000000000000000 ) ) ;
#9065 = DIRECTION ( 'NONE',  ( -1.000000000000000000, -0.000000000000000000, -0.000000000000000000 ) ) ;
#9066 = EDGE_LOOP ( 'NONE', ( #1054, #7662, #9063, #3789 ) ) ;
#9067 = CARTESIAN_POINT ( 'NONE',  ( 27.00000000000000355, 29.99999999999997158, 64.00000000000000000 ) ) ;
#9068 = ADVANCED_FACE ( 'NONE', ( #1774 ), #2552, .F. ) ;
#9069 = LINE ( 'NONE', #1682, #416 ) ;
#9070 = EDGE_CURVE ( 'NONE', #4478, #1970, #6416, .T. ) ;
#9071 = ORIENTED_EDGE ( 'NONE', *, *, #8827, .F. ) ;
#9072 = EDGE_LOOP ( 'NONE', ( #1366, #8283 ) ) ;
#9073 = CONTEXT_DEPENDENT_SHAPE_REPRESENTATION ( #329, #4230 ) ;
#9074 = CARTESIAN_POINT ( 'NONE',  ( -22.50000000000000355, 0.000000000000000000, 5.000000000000000000 ) ) ;
#9075 = AXIS2_PLACEMENT_3D ( 'NONE', #2379, #5307, #3673 ) ;
#9076 = DIRECTION ( 'NONE',  ( 1.000000000000000000, 0.000000000000000000, 0.000000000000000000 ) ) ;
#9077 = DIRECTION ( 'NONE',  ( -1.000000000000000000, 0.000000000000000000, 0.000000000000000000 ) ) ;
#9078 = DIRECTION ( 'NONE',  ( 0.000000000000000000, 0.000000000000000000, 1.000000000000000000 ) ) ;
#9079 = CARTESIAN_POINT ( 'NONE',  ( 5.000000000000000000, -14.14213562373112154, 15.70213562373564820 ) ) ;
#9080 = ORIENTED_EDGE ( 'NONE', *, *, #753, .F. ) ;
#9081 = ORIENTED_EDGE ( 'NONE', *, *, #3408, .F. ) ;
#9082 = CARTESIAN_POINT ( 'NONE',  ( -4.119968255444916849E-15, -3.500000000000000000, 0.000000000000000000 ) ) ;
#9083 = CARTESIAN_POINT ( 'NONE',  ( -6.000000000000000888, -22.50000000000000355, 2.000000000000013767 ) ) ;
#9084 = AXIS2_PLACEMENT_3D ( 'NONE', #1451, #6647, #2274 ) ;
#9085 = CARTESIAN_POINT ( 'NONE',  ( -53.29490495164537833, 18.67545040036925386, -90.28901569369799063 ) ) ;
#9086 = CARTESIAN_POINT ( 'NONE',  ( 0.7500000000000000000, -2.750000000000002665, 1.500000000000000000 ) ) ;
#9087 = ORIENTED_EDGE ( 'NONE', *, *, #6134, .F. ) ;
#9088 = VERTEX_POINT ( 'NONE', #3940 ) ;
#9089 = ORIENTED_EDGE ( 'NONE', *, *, #5679, .T. ) ;
#9090 =( NAMED_UNIT ( * ) SI_UNIT ( $, .STERADIAN. ) SOLID_ANGLE_UNIT ( ) );
#9091 = ORIENTED_EDGE ( 'NONE', *, *, #9436, .F. ) ;
#9092 = CARTESIAN_POINT ( 'NONE',  ( 53.29490495164537833, -27.56180520566615044, -41.61356529332876875 ) ) ;
#9093 = DIRECTION ( 'NONE',  ( -0.6785983445458488861, -0.2810846377148297770, -0.6785983445458412255 ) ) ;
#9094 = AXIS2_PLACEMENT_3D ( 'NONE', #6491, #1337, #7198 ) ;
#9095 = DIRECTION ( 'NONE',  ( -0.000000000000000000, -0.000000000000000000, -1.000000000000000000 ) ) ;
#9096 = DIRECTION ( 'NONE',  ( -1.000000000000000000, 0.000000000000000000, 0.000000000000000000 ) ) ;
#9097 = CYLINDRICAL_SURFACE ( 'NONE', #520, 3.000000000000002665 ) ;
#9098 = AXIS2_PLACEMENT_3D ( 'NONE', #5322, #8250, #7523 ) ;
#9099 = LINE ( 'NONE', #8293, #5744 ) ;
#9100 = ORIENTED_EDGE ( 'NONE', *, *, #7940, .F. ) ;
#9101 = EDGE_CURVE ( 'NONE', #2523, #4781, #2269, .T. ) ;
#9102 = ORIENTED_EDGE ( 'NONE', *, *, #4663, .F. ) ;
#9103 = CARTESIAN_POINT ( 'NONE',  ( 34.25000000000000000, 43.00000000000000000, -25.00000000000000000 ) ) ;
#9104 = EDGE_LOOP ( 'NONE', ( #4489, #8547, #2043, #1052, #4370, #461, #7978 ) ) ;
#9105 = EDGE_CURVE ( 'NONE', #3433, #2908, #8978, .T. ) ;
#9106 = DIRECTION ( 'NONE',  ( -0.000000000000000000, -0.000000000000000000, -1.000000000000000000 ) ) ;
#9107 = CARTESIAN_POINT ( 'NONE',  ( -0.7500000000000000000, 0.7500000000000000000, 0.000000000000000000 ) ) ;
#9108 = ADVANCED_FACE ( 'NONE', ( #2464 ), #6882, .F. ) ;
#9109 = ADVANCED_FACE ( 'NONE', ( #296 ), #7640, .F. ) ;
#9110 = EDGE_LOOP ( 'NONE', ( #7791, #5047, #624, #216, #3167, #9080 ) ) ;
#9111 = VECTOR ( 'NONE', #6481, 1000.000000000000000 ) ;
#9112 = CARTESIAN_POINT ( 'NONE',  ( 50.79490495164537833, -30.00000000000000355, -82.50000000000001421 ) ) ;
#9113 = DIRECTION ( 'NONE',  ( -0.000000000000000000, -0.000000000000000000, -1.000000000000000000 ) ) ;
#9114 = ORIENTED_EDGE ( 'NONE', *, *, #8243, .T. ) ;
#9115 = VECTOR ( 'NONE', #1310, 1000.000000000000000 ) ;
#9116 = VERTEX_POINT ( 'NONE', #1919 ) ;
#9117 = PRODUCT_CONTEXT ( 'NONE', #2785, 'mechanical' ) ;
#9118 = EDGE_CURVE ( 'NONE', #7922, #4458, #5953, .T. ) ;
#9119 = DIRECTION ( 'NONE',  ( -0.000000000000000000, -0.7071067811865455743, -0.7071067811865494601 ) ) ;
#9120 = VECTOR ( 'NONE', #3996, 1000.000000000000000 ) ;
#9121 = CARTESIAN_POINT ( 'NONE',  ( 1.571166602479410136E-13, -22.50000000000000355, 0.000000000000000000 ) ) ;
#9122 = FILL_AREA_STYLE_COLOUR ( '', #6486 ) ;
#9123 = DIRECTION ( 'NONE',  ( 0.000000000000000000, 0.000000000000000000, 1.000000000000000000 ) ) ;
#9124 = EDGE_CURVE ( 'NONE', #6180, #5267, #2114, .T. ) ;
#9125 = CARTESIAN_POINT ( 'NONE',  ( 37.00000000000000000, -21.98223304703364889, -86.98223304703364533 ) ) ;
#9126 = ORIENTED_EDGE ( 'NONE', *, *, #7958, .F. ) ;
#9127 = LINE ( 'NONE', #3590, #5649 ) ;
#9128 = ORIENTED_EDGE ( 'NONE', *, *, #8346, .F. ) ;
#9129 = CARTESIAN_POINT ( 'NONE',  ( 51.96152422706632734, 30.00000000000000000, -134.0000000000000284 ) ) ;
#9130 = FACE_OUTER_BOUND ( 'NONE', #4162, .T. ) ;
#9131 = LINE ( 'NONE', #2802, #4395 ) ;
#9132 = DIRECTION ( 'NONE',  ( -0.000000000000000000, -0.000000000000000000, -1.000000000000000000 ) ) ;
#9133 = ORIENTED_EDGE ( 'NONE', *, *, #4823, .F. ) ;
#9134 = ORIENTED_EDGE ( 'NONE', *, *, #7882, .T. ) ;
#9135 = SHAPE_REPRESENTATION_RELATIONSHIP ( 'NONE' , 'NONE' ,  #8501, #3701 ) ;
#9136 = ORIENTED_EDGE ( 'NONE', *, *, #3603, .T. ) ;
#9137 = CARTESIAN_POINT ( 'NONE',  ( 0.000000000000000000, 0.000000000000000000, 26.99999999999999289 ) ) ;
#9138 = DIRECTION ( 'NONE',  ( 1.000000000000000000, 0.000000000000000000, 0.000000000000000000 ) ) ;
#9139 = EDGE_CURVE ( 'NONE', #3367, #9386, #7483, .T. ) ;
#9140 = DIRECTION ( 'NONE',  ( -0.6785983445458478869, 0.2810846377148137898, 0.6785983445458488861 ) ) ;
#9141 = VECTOR ( 'NONE', #3629, 1000.000000000000000 ) ;
#9142 = AXIS2_PLACEMENT_3D ( 'NONE', #1316, #551, #5025 ) ;
#9143 = CARTESIAN_POINT ( 'NONE',  ( 31.00000000000002132, 0.000000000000000000, 32.00000000000000000 ) ) ;
#9144 = EDGE_CURVE ( 'NONE', #8767, #4339, #7780, .T. ) ;
#9145 = CARTESIAN_POINT ( 'NONE',  ( 0.000000000000000000, -34.99999999999999289, 32.00000000000000000 ) ) ;
#9146 = EDGE_LOOP ( 'NONE', ( #7558, #1744, #440, #4982 ) ) ;
#9147 = ORIENTED_EDGE ( 'NONE', *, *, #1831, .F. ) ;
#9148 = CARTESIAN_POINT ( 'NONE',  ( -30.00000000000000000, 0.000000000000000000, 2.999999999999999112 ) ) ;
#9149 = ORIENTED_EDGE ( 'NONE', *, *, #4548, .F. ) ;
#9150 = AXIS2_PLACEMENT_3D ( 'NONE', #8227, #3958, #925 ) ;
#9151 = DIRECTION ( 'NONE',  ( 1.000000000000000000, 0.000000000000000000, -0.000000000000000000 ) ) ;
#9152 = LINE ( 'NONE', #5382, #9170 ) ;
#9153 = ORIENTED_EDGE ( 'NONE', *, *, #1373, .F. ) ;
#9154 = AXIS2_PLACEMENT_3D ( 'NONE', #680, #3611, #6549 ) ;
#9155 = DIRECTION ( 'NONE',  ( -1.000000000000000000, 0.000000000000000000, 0.000000000000000000 ) ) ;
#9156 = AXIS2_PLACEMENT_3D ( 'NONE', #8123, #5858, #1529 ) ;
#9157 = VECTOR ( 'NONE', #4407, 1000.000000000000000 ) ;
#9158 = CONICAL_SURFACE ( 'NONE', #3962, 6.000000000000000888, 0.7853981633974498333 ) ;
#9159 = CARTESIAN_POINT ( 'NONE',  ( 53.29490495164537833, -27.56180520566615044, -81.40266088840111536 ) ) ;
#9160 = CARTESIAN_POINT ( 'NONE',  ( -5.088821267330767562, -27.44505377838575200, 0.9111060003908462157 ) ) ;
#9161 = AXIS2_PLACEMENT_3D ( 'NONE', #2968, #9155, #467 ) ;
#9162 = ORIENTED_EDGE ( 'NONE', *, *, #6896, .T. ) ;
#9163 = ORIENTED_EDGE ( 'NONE', *, *, #9026, .F. ) ;
#9164 = AXIS2_PLACEMENT_3D ( 'NONE', #4402, #3733, #1150 ) ;
#9165 = CIRCLE ( 'NONE', #5034, 6.000000000000001776 ) ;
#9166 = ADVANCED_FACE ( 'NONE', ( #6257 ), #8408, .T. ) ;
#9167 =( BOUNDED_CURVE ( )  B_SPLINE_CURVE ( 3, ( #5456, #979, #3914, #9092 ),
 .UNSPECIFIED., .F., .F. ) 
 B_SPLINE_CURVE_WITH_KNOTS ( ( 4, 4 ),
 ( 0.000000000000000000, 0.4772783968222097384 ),
 .UNSPECIFIED. ) 
 CURVE ( )  GEOMETRIC_REPRESENTATION_ITEM ( )  RATIONAL_B_SPLINE_CURVE ( ( 1.000000000000000000, 0.9811070276743185659, 0.9811070276743185659, 1.000000000000000000 ) ) 
 REPRESENTATION_ITEM ( '' )  );
#9168 = DIRECTION ( 'NONE',  ( 0.000000000000000000, 0.000000000000000000, 1.000000000000000000 ) ) ;
#9169 = EDGE_CURVE ( 'NONE', #9251, #8566, #3035, .T. ) ;
#9170 = VECTOR ( 'NONE', #6100, 1000.000000000000000 ) ;
#9171 = FACE_OUTER_BOUND ( 'NONE', #3037, .T. ) ;
#9172 = CARTESIAN_POINT ( 'NONE',  ( 3.000000000000000000, -22.50000000000000355, 10.00000000000000000 ) ) ;
#9173 = CARTESIAN_POINT ( 'NONE',  ( -28.75000000000002842, 0.6738334415499688257, 1.750000000000029754 ) ) ;
#9174 = EDGE_LOOP ( 'NONE', ( #7333, #976 ) ) ;
#9175 = FACE_OUTER_BOUND ( 'NONE', #3818, .T. ) ;
#9176 = CIRCLE ( 'NONE', #5191, 1.560000000000000719 ) ;
#9177 = CIRCLE ( 'NONE', #1825, 1.560000000001265263 ) ;
#9178 = VERTEX_POINT ( 'NONE', #2602 ) ;
#9179 = VECTOR ( 'NONE', #7160, 1000.000000000000000 ) ;
#9180 = CARTESIAN_POINT ( 'NONE',  ( -31.99999999999999289, 35.00000000000000000, 64.00000000000000000 ) ) ;
#9181 = EDGE_CURVE ( 'NONE', #6631, #2860, #1146, .T. ) ;
#9182 = CARTESIAN_POINT ( 'NONE',  ( 22.50000000000000355, 0.000000000000000000, 5.000000000000000000 ) ) ;
#9183 = CYLINDRICAL_SURFACE ( 'NONE', #5975, 3.000000000000002665 ) ;
#9184 = DIRECTION ( 'NONE',  ( -1.000000000000000000, 0.000000000000000000, 0.000000000000000000 ) ) ;
#9185 = AXIS2_PLACEMENT_3D ( 'NONE', #5533, #5439, #1779 ) ;
#9186 = EDGE_LOOP ( 'NONE', ( #7833, #7142, #4421, #5959 ) ) ;
#9187 = ORIENTED_EDGE ( 'NONE', *, *, #5666, .F. ) ;
#9188 = ORIENTED_EDGE ( 'NONE', *, *, #4596, .T. ) ;
#9189 = CARTESIAN_POINT ( 'NONE',  ( 22.50000000000000355, 0.000000000000000000, 2.000000000000035083 ) ) ;
#9190 = CARTESIAN_POINT ( 'NONE',  ( 0.000000000000000000, -34.00000000000001421, 32.00000000000000000 ) ) ;
#9191 = CARTESIAN_POINT ( 'NONE',  ( 37.00000000000000000, 15.90990257669733943, -54.09009742330271564 ) ) ;
#9192 = CARTESIAN_POINT ( 'NONE',  ( -51.96152422706631313, 30.00000000000000711, -12.99999999999999289 ) ) ;
#9193 = CARTESIAN_POINT ( 'NONE',  ( 5.000000000000000000, -9.628187502531647418E-13, -18.43999999999823913 ) ) ;
#9194 = ORIENTED_EDGE ( 'NONE', *, *, #5242, .T. ) ;
#9195 = ORIENTED_EDGE ( 'NONE', *, *, #1517, .T. ) ;
#9196 = AXIS2_PLACEMENT_3D ( 'NONE', #4680, #1020, #6893 ) ;
#9197 = EDGE_LOOP ( 'NONE', ( #1129, #4148 ) ) ;
#9198 = DIRECTION ( 'NONE',  ( 1.000000000000000000, 1.776356839400250465E-15, 0.000000000000000000 ) ) ;
#9199 = ORIENTED_EDGE ( 'NONE', *, *, #1341, .T. ) ;
#9200 = DIRECTION ( 'NONE',  ( 1.000000000000000000, 0.000000000000000000, 0.000000000000000000 ) ) ;
#9201 = CARTESIAN_POINT ( 'NONE',  ( 18.50000000000001776, 2.265596578422605368E-15, 0.000000000000000000 ) ) ;
#9202 = DIRECTION ( 'NONE',  ( 1.000000000000000000, 0.000000000000000000, 0.000000000000000000 ) ) ;
#9203 = AXIS2_PLACEMENT_3D ( 'NONE', #5317, #6040, #8105 ) ;
#9204 = FACE_OUTER_BOUND ( 'NONE', #3065, .T. ) ;
#9205 = ORIENTED_EDGE ( 'NONE', *, *, #5243, .F. ) ;
#9206 = ORIENTED_EDGE ( 'NONE', *, *, #8290, .F. ) ;
#9207 = APPLICATION_PROTOCOL_DEFINITION ( 'draft international standard', 'automotive_design', 1998, #1478 ) ;
#9208 = EDGE_CURVE ( 'NONE', #8845, #4499, #8714, .T. ) ;
#9209 = VECTOR ( 'NONE', #3200, 999.9999999999998863 ) ;
#9210 = CARTESIAN_POINT ( 'NONE',  ( 53.29490495164537833, -15.90990257669733943, -85.90990257669729147 ) ) ;
#9211 = DIRECTION ( 'NONE',  ( -0.7071067811865509034, -0.7071067811865442421, 0.000000000000000000 ) ) ;
#9212 = DIRECTION ( 'NONE',  ( 0.6785983445458459995, 0.2810846377148253916, -0.6785983445458459995 ) ) ;
#9213 = PLANE ( 'NONE',  #2723 ) ;
#9214 = ORIENTED_EDGE ( 'NONE', *, *, #8815, .T. ) ;
#9215 = ORIENTED_EDGE ( 'NONE', *, *, #553, .F. ) ;
#9216 = EDGE_CURVE ( 'NONE', #3965, #8532, #2583, .T. ) ;
#9217 =( BOUNDED_CURVE ( )  B_SPLINE_CURVE ( 3, ( #3149, #7712, #6989, #4017 ),
 .UNSPECIFIED., .F., .T. ) 
 B_SPLINE_CURVE_WITH_KNOTS ( ( 4, 4 ),
 ( 3.141592653589793116, 3.926990816987241395 ),
 .UNSPECIFIED. ) 
 CURVE ( )  GEOMETRIC_REPRESENTATION_ITEM ( )  RATIONAL_B_SPLINE_CURVE ( ( 1.000000000000000000, 0.9492530216741911220, 0.9492530216741911220, 1.000000000000000000 ) ) 
 REPRESENTATION_ITEM ( '' )  );
#9218 = VERTEX_POINT ( 'NONE', #6862 ) ;
#9219 = ADVANCED_FACE ( 'NONE', ( #6149 ), #7948, .T. ) ;
#9220 = DIRECTION ( 'NONE',  ( 0.000000000000000000, 0.000000000000000000, -1.000000000000000000 ) ) ;
#9221 = EDGE_CURVE ( 'NONE', #7742, #2498, #9165, .T. ) ;
#9222 = ADVANCED_FACE ( 'NONE', ( #1042 ), #185, .F. ) ;
#9223 = DIRECTION ( 'NONE',  ( 0.000000000000000000, 0.000000000000000000, 1.000000000000000000 ) ) ;
#9224 = CYLINDRICAL_SURFACE ( 'NONE', #8875, 11.00000000000000711 ) ;
#9225 = CARTESIAN_POINT ( 'NONE',  ( -37.22467645238203460, -47.05659850664382304, -5.608807313787673721 ) ) ;
#9226 = CARTESIAN_POINT ( 'NONE',  ( -60.00000000000000000, 60.00000000000000000, 0.000000000000000000 ) ) ;
#9227 = ORIENTED_EDGE ( 'NONE', *, *, #3589, .F. ) ;
#9228 = ORIENTED_EDGE ( 'NONE', *, *, #6271, .T. ) ;
#9229 = CARTESIAN_POINT ( 'NONE',  ( 7.219041098785732302, 80.45324141007795049, 113.9561622983770519 ) ) ;
#9230 = ORIENTED_EDGE ( 'NONE', *, *, #7060, .T. ) ;
#9231 = EDGE_CURVE ( 'NONE', #955, #6124, #4729, .T. ) ;
#9232 = FACE_BOUND ( 'NONE', #7035, .T. ) ;
#9233 = EDGE_CURVE ( 'NONE', #5080, #6587, #2866, .T. ) ;
#9234 = CARTESIAN_POINT ( 'NONE',  ( -27.16490240584776572, 3.793344078502526973, 0.4263419363949844110 ) ) ;
#9235 = ADVANCED_FACE ( 'NONE', ( #1859 ), #5325, .F. ) ;
#9236 = CARTESIAN_POINT ( 'NONE',  ( -31.99999999999999289, 35.00000000000000000, 5.000000000000004441 ) ) ;
#9237 = LINE ( 'NONE', #2039, #2061 ) ;
#9238 = CIRCLE ( 'NONE', #1733, 1.000000000000000000 ) ;
#9239 = FACE_OUTER_BOUND ( 'NONE', #8590, .T. ) ;
#9240 = EDGE_LOOP ( 'NONE', ( #6659, #7237, #378, #2066, #6813, #7462 ) ) ;
#9241 = ORIENTED_EDGE ( 'NONE', *, *, #1335, .F. ) ;
#9242 = DIRECTION ( 'NONE',  ( 1.000000000000000000, 0.000000000000000000, 0.000000000000000000 ) ) ;
#9243 = ORIENTED_EDGE ( 'NONE', *, *, #7231, .F. ) ;
#9244 = CARTESIAN_POINT ( 'NONE',  ( -16.50000000000000000, 7.347880794884123680E-16, 5.000000000000000000 ) ) ;
#9245 = LINE ( 'NONE', #6334, #5909 ) ;
#9246 = DIRECTION ( 'NONE',  ( 0.000000000000000000, 0.000000000000000000, -1.000000000000000000 ) ) ;
#9247 = CARTESIAN_POINT ( 'NONE',  ( -26.99999999999998934, 0.000000000000000000, 64.00000000000000000 ) ) ;
#9248 = CIRCLE ( 'NONE', #3269, 14.49999999999998401 ) ;
#9249 = DIRECTION ( 'NONE',  ( -1.000000000000000000, 0.000000000000000000, 0.000000000000000000 ) ) ;
#9250 = CARTESIAN_POINT ( 'NONE',  ( 12.37436867076458036, -12.37436867076458036, 44.37436867076458213 ) ) ;
#9251 = VERTEX_POINT ( 'NONE', #4649 ) ;
#9252 = ORIENTED_EDGE ( 'NONE', *, *, #3828, .T. ) ;
#9253 = ITEM_DEFINED_TRANSFORMATION ( 'NONE', 'NONE', #4383,  #1614 ) ;
#9254 = EDGE_CURVE ( 'NONE', #5515, #1435, #4024, .T. ) ;
#9255 = AXIS2_PLACEMENT_3D ( 'NONE', #3538, #9294, #3440 ) ;
#9256 = DIRECTION ( 'NONE',  ( 0.000000000000000000, 0.000000000000000000, -1.000000000000000000 ) ) ;
#9257 = VECTOR ( 'NONE', #5272, 1000.000000000000000 ) ;
#9258 = LINE ( 'NONE', #5723, #4805 ) ;
#9259 = CARTESIAN_POINT ( 'NONE',  ( 7.180166011355011868, 26.02777777777776791, 0.000000000000000000 ) ) ;
#9260 = ORIENTED_EDGE ( 'NONE', *, *, #774, .T. ) ;
#9261 = VERTEX_POINT ( 'NONE', #9148 ) ;
#9262 = VERTEX_POINT ( 'NONE', #2586 ) ;
#9263 = CIRCLE ( 'NONE', #8964, 15.00000000000000000 ) ;
#9264 = ORIENTED_EDGE ( 'NONE', *, *, #4245, .F. ) ;
#9265 = CARTESIAN_POINT ( 'NONE',  ( 41.99999999999997868, -12.50000000000000355, -100.0000000000000000 ) ) ;
#9266 = AXIS2_PLACEMENT_3D ( 'NONE', #4802, #5624, #5847 ) ;
#9267 = LINE ( 'NONE', #7159, #5491 ) ;
#9268 = LINE ( 'NONE', #2119, #5529 ) ;
#9269 = DIRECTION ( 'NONE',  ( -0.000000000000000000, -0.000000000000000000, -1.000000000000000000 ) ) ;
#9270 = ADVANCED_FACE ( 'NONE', ( #2536, #5516 ), #282, .T. ) ;
#9271 = DIRECTION ( 'NONE',  ( 1.000000000000000000, 0.000000000000000000, 0.000000000000000000 ) ) ;
#9272 = ORIENTED_EDGE ( 'NONE', *, *, #7943, .F. ) ;
#9273 = ORIENTED_EDGE ( 'NONE', *, *, #6358, .F. ) ;
#9274 = DIRECTION ( 'NONE',  ( -1.000000000000000000, 0.000000000000000000, 0.000000000000000000 ) ) ;
#9275 = ORIENTED_EDGE ( 'NONE', *, *, #368, .T. ) ;
#9276 = PRODUCT_DEFINITION_FORMATION_WITH_SPECIFIED_SOURCE ( 'ANY', '', #2705, .NOT_KNOWN. ) ;
#9277 = CARTESIAN_POINT ( 'NONE',  ( 0.000000000000000000, -22.50000000000000355, 10.00000000000000000 ) ) ;
#9278 = FACE_OUTER_BOUND ( 'NONE', #7765, .T. ) ;
#9280 = EDGE_CURVE ( 'NONE', #4271, #6932, #6046, .T. ) ;
#9279 = DIRECTION ( 'NONE',  ( -0.000000000000000000, -0.000000000000000000, -1.000000000000000000 ) ) ;
#9281 = DIRECTION ( 'NONE',  ( 0.000000000000000000, 0.000000000000000000, 1.000000000000000000 ) ) ;
#9282 = AXIS2_PLACEMENT_3D ( 'NONE', #7818, #6431, #6477 ) ;
#9283 = CARTESIAN_POINT ( 'NONE',  ( 0.000000000000000000, 22.50000000000000355, 10.00000000000000000 ) ) ;
#9284 = PRODUCT_DEFINITION_SHAPE ( 'NONE', 'NONE',  #9496 ) ;
#9285 = EDGE_LOOP ( 'NONE', ( #601, #3195 ) ) ;
#9286 = ORIENTED_EDGE ( 'NONE', *, *, #7344, .F. ) ;
#9287 = EDGE_CURVE ( 'NONE', #6094, #1673, #8446, .T. ) ;
#9288 = DIRECTION ( 'NONE',  ( -0.000000000000000000, -0.000000000000000000, -1.000000000000000000 ) ) ;
#9289 = EDGE_LOOP ( 'NONE', ( #4067, #4662 ) ) ;
#9290 = CARTESIAN_POINT ( 'NONE',  ( -19.74999999999999645, 43.00000000000000000, -25.00000000000000000 ) ) ;
#9291 = DIRECTION ( 'NONE',  ( 0.000000000000000000, 0.000000000000000000, -1.000000000000000000 ) ) ;
#9292 = DIRECTION ( 'NONE',  ( -0.5773502691896249539, -0.5773502691896263972, 0.5773502691896258421 ) ) ;
#9293 = CARTESIAN_POINT ( 'NONE',  ( 0.000000000000000000, 22.50000000000000355, 15.00000000000000000 ) ) ;
#9294 = DIRECTION ( 'NONE',  ( 0.000000000000000000, 0.000000000000000000, -1.000000000000000000 ) ) ;
#9295 = CARTESIAN_POINT ( 'NONE',  ( -37.73845885098648978, 45.76160744848121453, -6.169970105658134862 ) ) ;
#9296 = CIRCLE ( 'NONE', #4706, 1.560000000000002274 ) ;
#9297 = EDGE_LOOP ( 'NONE', ( #5586, #8096, #5070, #5860 ) ) ;
#9298 = ORIENTED_EDGE ( 'NONE', *, *, #7837, .F. ) ;
#9299 = CONTEXT_DEPENDENT_SHAPE_REPRESENTATION ( #9336, #2246 ) ;
#9300 = VECTOR ( 'NONE', #7435, 999.9999999999998863 ) ;
#9301 = AXIS2_PLACEMENT_3D ( 'NONE', #4624, #4215, #4317 ) ;
#9302 = FACE_OUTER_BOUND ( 'NONE', #8056, .T. ) ;
#9303 = AXIS2_PLACEMENT_3D ( 'NONE', #7655, #4628, #5304 ) ;
#9304 = CARTESIAN_POINT ( 'NONE',  ( 2.143131898507868248E-15, 34.00000000000001421, 14.49999999999999822 ) ) ;
#9305 = VECTOR ( 'NONE', #3202, 1000.000000000000000 ) ;
#9306 = CARTESIAN_POINT ( 'NONE',  ( 1.571166602479410136E-13, -22.50000000000000355, 15.00000000000000000 ) ) ;
#9307 = DIRECTION ( 'NONE',  ( -1.000000000000000000, -0.000000000000000000, -0.000000000000000000 ) ) ;
#9308 = CIRCLE ( 'NONE', #4727, 17.50000000000000000 ) ;
#9309 = ORIENTED_EDGE ( 'NONE', *, *, #6356, .F. ) ;
#9310 = EDGE_LOOP ( 'NONE', ( #7053, #7116, #2560, #9039, #7120, #3587 ) ) ;
#9311 = CONICAL_SURFACE ( 'NONE', #8861, 2.499999999999998668, 0.7853981633974461696 ) ;
#9312 = ADVANCED_FACE ( 'NONE', ( #945 ), #4789, .F. ) ;
#9313 = VERTEX_POINT ( 'NONE', #6911 ) ;
#9314 = CIRCLE ( 'NONE', #5181, 8.000000000000047962 ) ;
#9315 = ORIENTED_EDGE ( 'NONE', *, *, #2004, .F. ) ;
#9316 = EDGE_CURVE ( 'NONE', #2688, #6912, #322, .T. ) ;
#9317 = CARTESIAN_POINT ( 'NONE',  ( 37.00000000000000000, -3.673940397442057600E-15, -70.00000000000000000 ) ) ;
#9318 = CIRCLE ( 'NONE', #5954, 0.7499999999986606269 ) ;
#9319 = DIRECTION ( 'NONE',  ( 0.000000000000000000, 0.000000000000000000, 1.000000000000000000 ) ) ;
#9320 = EDGE_CURVE ( 'NONE', #7086, #3688, #1810, .T. ) ;
#9321 = FACE_OUTER_BOUND ( 'NONE', #5037, .T. ) ;
#9322 = CARTESIAN_POINT ( 'NONE',  ( -28.40723282374007752, -2.660173739710364416, 1.529649672404344241 ) ) ;
#9323 = DIRECTION ( 'NONE',  ( 0.000000000000000000, 0.000000000000000000, 1.000000000000000000 ) ) ;
#9324 = AXIS2_PLACEMENT_3D ( 'NONE', #4165, #3531, #7090 ) ;
#9325 = ORIENTED_EDGE ( 'NONE', *, *, #6833, .T. ) ;
#9326 = ORIENTED_EDGE ( 'NONE', *, *, #3548, .F. ) ;
#9327 = DIRECTION ( 'NONE',  ( -0.5469441386040181374, -0.01989630609932445740, -0.8369326414056931229 ) ) ;
#9328 = EDGE_LOOP ( 'NONE', ( #3980, #4283 ) ) ;
#9329 = DIRECTION ( 'NONE',  ( 0.000000000000000000, 1.000000000000000000, 0.000000000000000000 ) ) ;
#9330 = ADVANCED_FACE ( 'NONE', ( #6812 ), #4068, .T. ) ;
#9331 = CARTESIAN_POINT ( 'NONE',  ( -17.49999999999999645, -4.703319286132082944, 14.49999999999999822 ) ) ;
#9332 = CIRCLE ( 'NONE', #1977, 1.560000000001265263 ) ;
#9333 = CARTESIAN_POINT ( 'NONE',  ( 5.000000000000000000, 14.14213562373247868, 15.70213562373191962 ) ) ;
#9334 = VECTOR ( 'NONE', #169, 1000.000000000000000 ) ;
#9335 = CARTESIAN_POINT ( 'NONE',  ( 60.00000000000000000, 7.347880794884118356E-15, 25.00000000000000000 ) ) ;
#9336 =( REPRESENTATION_RELATIONSHIP ('NONE','NONE', #1933, #8501 ) REPRESENTATION_RELATIONSHIP_WITH_TRANSFORMATION ( #4174 )SHAPE_REPRESENTATION_RELATIONSHIP( ) );
#9337 = CARTESIAN_POINT ( 'NONE',  ( 0.000000000000000000, -14.14213562373112154, 12.58213562373271621 ) ) ;
#9338 = EDGE_LOOP ( 'NONE', ( #2064, #9194, #3614, #7647 ) ) ;
#9339 = EDGE_CURVE ( 'NONE', #8518, #55, #4254, .T. ) ;
#9340 = VERTEX_POINT ( 'NONE', #7180 ) ;
#9341 = CARTESIAN_POINT ( 'NONE',  ( -2.081312099201802823, 28.14194242914269495, 1.216216932313278098 ) ) ;
#9342 = ORIENTED_EDGE ( 'NONE', *, *, #4297, .F. ) ;
#9343 = EDGE_CURVE ( 'NONE', #7585, #3888, #7204, .T. ) ;
#9344 = DIRECTION ( 'NONE',  ( 0.000000000000000000, 0.7071067811865493491, 0.7071067811865455743 ) ) ;
#9345 = EDGE_CURVE ( 'NONE', #1435, #6513, #8687, .T. ) ;
#9346 = DIRECTION ( 'NONE',  ( 1.000000000000000000, 0.000000000000000000, 0.000000000000000000 ) ) ;
#9347 = FACE_OUTER_BOUND ( 'NONE', #183, .T. ) ;
#9348 = ADVANCED_FACE ( 'NONE', ( #4880 ), #2773, .F. ) ;
#9349 = CARTESIAN_POINT ( 'NONE',  ( -30.00000000000000000, 0.000000000000000000, 10.00000000000000000 ) ) ;
#9350 = AXIS2_PLACEMENT_3D ( 'NONE', #4516, #8888, #8171 ) ;
#9351 = CARTESIAN_POINT ( 'NONE',  ( 2.818925648462311528E-15, 3.500000000000000000, 0.000000000000000000 ) ) ;
#9352 = CARTESIAN_POINT ( 'NONE',  ( 4.703319286132082944, -17.49999999999999645, 49.50000000000000000 ) ) ;
#9353 = EDGE_LOOP ( 'NONE', ( #7617, #2883, #3743, #6689 ) ) ;
#9354 = ORIENTED_EDGE ( 'NONE', *, *, #4006, .F. ) ;
#9355 = DIRECTION ( 'NONE',  ( -1.000000000000000000, -0.000000000000000000, -0.000000000000000000 ) ) ;
#9356 = CONTEXT_DEPENDENT_SHAPE_REPRESENTATION ( #2955, #4389 ) ;
#9357 = EDGE_CURVE ( 'NONE', #3807, #2599, #3526, .T. ) ;
#9358 = ADVANCED_FACE ( 'NONE', ( #7132 ), #5565, .F. ) ;
#9359 = CARTESIAN_POINT ( 'NONE',  ( 60.00000000000000000, 7.347880794884118356E-15, -30.00000000000000000 ) ) ;
#9361 = EDGE_CURVE ( 'NONE', #943, #7855, #1265, .T. ) ;
#9360 = DIRECTION ( 'NONE',  ( 0.7071067811865494601, 0.000000000000000000, -0.7071067811865455743 ) ) ;
#9362 = CARTESIAN_POINT ( 'NONE',  ( 5.000000000000000000, 7.653668647302530381, 19.22759065022631830 ) ) ;
#9363 = DIRECTION ( 'NONE',  ( 0.000000000000000000, 0.000000000000000000, 1.000000000000000000 ) ) ;
#9364 = ORIENTED_EDGE ( 'NONE', *, *, #8816, .T. ) ;
#9365 = EDGE_LOOP ( 'NONE', ( #8114, #3991 ) ) ;
#9366 = VERTEX_POINT ( 'NONE', #6473 ) ;
#9367 = AXIS2_PLACEMENT_3D ( 'NONE', #8495, #6336, #4840 ) ;
#9368 = VERTEX_POINT ( 'NONE', #6291 ) ;
#9369 = DIRECTION ( 'NONE',  ( -0.000000000000000000, -0.000000000000000000, -1.000000000000000000 ) ) ;
#9370 = FACE_BOUND ( 'NONE', #6909, .T. ) ;
#9371 = CARTESIAN_POINT ( 'NONE',  ( 0.000000000000000000, 20.00000000000120437, 7.412591687719288072E-13 ) ) ;
#9372 = PRODUCT_DEFINITION_SHAPE ( 'NONE', 'NONE',  #9477 ) ;
#9373 = CARTESIAN_POINT ( 'NONE',  ( -28.10782586465402133, -3.612161042402820765, 1.337173770134741924 ) ) ;
#9374 = FACE_BOUND ( 'NONE', #1202, .T. ) ;
#9375 = ORIENTED_EDGE ( 'NONE', *, *, #5104, .F. ) ;
#9376 = CARTESIAN_POINT ( 'NONE',  ( -17.50000000000000355, 2.143131898507868643E-15, 14.49999999999999822 ) ) ;
#9377 = ORIENTED_EDGE ( 'NONE', *, *, #6654, .T. ) ;
#9378 = AXIS2_PLACEMENT_3D ( 'NONE', #3812, #6755, #4585 ) ;
#9379 = FACE_BOUND ( 'NONE', #6577, .T. ) ;
#9380 = LINE ( 'NONE', #593, #4236 ) ;
#9381 = EDGE_CURVE ( 'NONE', #2690, #1211, #4202, .T. ) ;
#9382 = CARTESIAN_POINT ( 'NONE',  ( 37.73845885098648978, 45.76160744848121453, -6.169970105658139303 ) ) ;
#9383 = DIRECTION ( 'NONE',  ( 0.5773502691896252870, 0.5773502691896258421, 0.5773502691896261751 ) ) ;
#9384 = CIRCLE ( 'NONE', #5253, 2.499999999999998668 ) ;
#9385 = CARTESIAN_POINT ( 'NONE',  ( -2.060470863509831219, -28.13894063079882457, 1.213559982044000840 ) ) ;
#9386 = VERTEX_POINT ( 'NONE', #5612 ) ;
#9387 = EDGE_LOOP ( 'NONE', ( #6340, #4993 ) ) ;
#9388 = DIRECTION ( 'NONE',  ( 1.000000000000000000, 0.000000000000000000, 0.000000000000000000 ) ) ;
#9389 = AXIS2_PLACEMENT_3D ( 'NONE', #5152, #9427, #6693 ) ;
#9390 = ORIENTED_EDGE ( 'NONE', *, *, #7764, .F. ) ;
#9391 = CYLINDRICAL_SURFACE ( 'NONE', #1513, 15.00000000000000000 ) ;
#9392 = LINE ( 'NONE', #8625, #5354 ) ;
#9393 = DIRECTION ( 'NONE',  ( 1.000000000000000000, 0.000000000000000000, 0.000000000000000000 ) ) ;
#9394 = DIRECTION ( 'NONE',  ( 1.000000000000000000, 0.000000000000000000, 0.000000000000000000 ) ) ;
#9395 = AXIS2_PLACEMENT_3D ( 'NONE', #6076, #3228, #6891 ) ;
#9396 = EDGE_CURVE ( 'NONE', #8464, #287, #8670, .T. ) ;
#9397 = DIRECTION ( 'NONE',  ( 0.000000000000000000, 0.000000000000000000, -1.000000000000000000 ) ) ;
#9398 = DIRECTION ( 'NONE',  ( -0.000000000000000000, -0.000000000000000000, 1.000000000000000000 ) ) ;
#9399 = EDGE_CURVE ( 'NONE', #7970, #3755, #8534, .T. ) ;
#9400 = VERTEX_POINT ( 'NONE', #1951 ) ;
#9401 = ORIENTED_EDGE ( 'NONE', *, *, #5536, .T. ) ;
#9402 = EDGE_CURVE ( 'NONE', #2584, #6427, #8489, .T. ) ;
#9403 = EDGE_CURVE ( 'NONE', #2622, #7382, #4841, .T. ) ;
#9404 = DIRECTION ( 'NONE',  ( 0.000000000000000000, 0.7071067811865477948, -0.7071067811865473507 ) ) ;
#9405 = CIRCLE ( 'NONE', #3574, 15.00000000000000000 ) ;
#9406 = LINE ( 'NONE', #8014, #119 ) ;
#9407 = LINE ( 'NONE', #5767, #2198 ) ;
#9408 = CARTESIAN_POINT ( 'NONE',  ( 0.000000000000000000, 0.000000000000000000, 0.000000000000000000 ) ) ;
#9409 = EDGE_LOOP ( 'NONE', ( #7201, #5983 ) ) ;
#9410 = VECTOR ( 'NONE', #8619, 1000.000000000000000 ) ;
#9411 = EDGE_LOOP ( 'NONE', ( #7625, #3391, #1173, #281 ) ) ;
#9412 = ORIENTED_EDGE ( 'NONE', *, *, #3222, .F. ) ;
#9413 = VERTEX_POINT ( 'NONE', #3477 ) ;
#9414 = ADVANCED_FACE ( 'NONE', ( #6426, #2044 ), #4834, .T. ) ;
#9415 = CONICAL_SURFACE ( 'NONE', #4362, 18.49999999999998934, 0.7853981633974517207 ) ;
#9416 = DIRECTION ( 'NONE',  ( -1.000000000000000000, 0.000000000000000000, 0.000000000000000000 ) ) ;
#9417 = CARTESIAN_POINT ( 'NONE',  ( 53.29490495164537833, 27.56180520566615044, -81.40266088840108694 ) ) ;
#9418 = CARTESIAN_POINT ( 'NONE',  ( 27.00000000000000000, -43.00000000000000000, 11.99999999999999645 ) ) ;
#9419 = EDGE_CURVE ( 'NONE', #4476, #410, #8180, .T. ) ;
#9420 = CARTESIAN_POINT ( 'NONE',  ( -28.75000000000003553, -0.3373484206894374338, 1.750000000000030642 ) ) ;
#9421 = AXIS2_PLACEMENT_3D ( 'NONE', #6523, #5848, #2960 ) ;
#9422 = DIRECTION ( 'NONE',  ( 0.7071067811865455743, 9.614813431917869865E-16, 0.7071067811865493491 ) ) ;
#9423 = ORIENTED_EDGE ( 'NONE', *, *, #4886, .F. ) ;
#9424 = DIRECTION ( 'NONE',  ( 0.000000000000000000, 0.000000000000000000, -1.000000000000000000 ) ) ;
#9425 = VECTOR ( 'NONE', #6420, 1000.000000000000000 ) ;
#9426 = VERTEX_POINT ( 'NONE', #7224 ) ;
#9427 = DIRECTION ( 'NONE',  ( 0.000000000000000000, 0.000000000000000000, -1.000000000000000000 ) ) ;
#9428 = CYLINDRICAL_SURFACE ( 'NONE', #5788, 0.7499999999986606269 ) ;
#9429 = CARTESIAN_POINT ( 'NONE',  ( 28.61406079152380144, 10.49089634068024068, -86.61406079152378368 ) ) ;
#9430 = CARTESIAN_POINT ( 'NONE',  ( 37.22467645238199196, 47.05659850664387278, -5.608807313787652404 ) ) ;
#9431 = DIRECTION ( 'NONE',  ( -1.000000000000000000, 0.000000000000000000, 0.000000000000000000 ) ) ;
#9432 = ORIENTED_EDGE ( 'NONE', *, *, #9208, .T. ) ;
#9433 = AXIS2_PLACEMENT_3D ( 'NONE', #7574, #8339, #1762 ) ;
#9434 = ORIENTED_EDGE ( 'NONE', *, *, #7924, .F. ) ;
#9435 = VERTEX_POINT ( 'NONE', #3576 ) ;
#9436 = EDGE_CURVE ( 'NONE', #2348, #1368, #1457, .T. ) ;
#9437 = CARTESIAN_POINT ( 'NONE',  ( -26.64999999999995950, -4.333301281932866900, 0.000000000000000000 ) ) ;
#9438 = CARTESIAN_POINT ( 'NONE',  ( -37.00000000000000000, -30.00000000000000000, -95.00000000000000000 ) ) ;
#9439 = DIRECTION ( 'NONE',  ( -1.000000000000000000, 0.000000000000000000, 0.000000000000000000 ) ) ;
#9440 = DIRECTION ( 'NONE',  ( 0.000000000000000000, -0.7071067811865456854, -0.7071067811865493491 ) ) ;
#9441 = AXIS2_PLACEMENT_3D ( 'NONE', #8478, #1892, #7847 ) ;
#9442 = EDGE_CURVE ( 'NONE', #1701, #4799, #3624, .T. ) ;
#9443 = DIRECTION ( 'NONE',  ( -1.000000000000000000, 0.000000000000000000, 0.000000000000000000 ) ) ;
#9444 = LINE ( 'NONE', #702, #7635 ) ;
#9445 = ORIENTED_EDGE ( 'NONE', *, *, #6871, .F. ) ;
#9446 = EDGE_LOOP ( 'NONE', ( #7078, #7133 ) ) ;
#9447 = LINE ( 'NONE', #8059, #8249 ) ;
#9448 = PRODUCT ( '5-Cover', '5-Cover', '', ( #3844 ) ) ;
#9449 = LINE ( 'NONE', #3549, #881 ) ;
#9450 = CIRCLE ( 'NONE', #861, 17.50000000000000000 ) ;
#9451 = VECTOR ( 'NONE', #2815, 1000.000000000000000 ) ;
#9452 = DIRECTION ( 'NONE',  ( 1.000000000000000000, 8.881784197001252323E-16, 0.000000000000000000 ) ) ;
#9453 = CARTESIAN_POINT ( 'NONE',  ( 0.000000000000000000, 0.000000000000000000, 50.00000000000000000 ) ) ;
#9454 = EDGE_LOOP ( 'NONE', ( #6800, #6761 ) ) ;
#9455 = ORIENTED_EDGE ( 'NONE', *, *, #2941, .F. ) ;
#9456 = ORIENTED_EDGE ( 'NONE', *, *, #1554, .F. ) ;
#9457 = EDGE_CURVE ( 'NONE', #1701, #8041, #6553, .T. ) ;
#9458 = AXIS2_PLACEMENT_3D ( 'NONE', #5059, #1498, #5741 ) ;
#9459 = VERTEX_POINT ( 'NONE', #1560 ) ;
#9460 = EDGE_CURVE ( 'NONE', #7998, #3455, #404, .T. ) ;
#9461 = AXIS2_PLACEMENT_3D ( 'NONE', #5013, #2672, #2855 ) ;
#9462 = LINE ( 'NONE', #98, #1311 ) ;
#9463 = DIRECTION ( 'NONE',  ( 1.000000000000000000, 0.000000000000000000, -0.000000000000000000 ) ) ;
#9464 = CIRCLE ( 'NONE', #1489, 6.000000000000001776 ) ;
#9465 = CARTESIAN_POINT ( 'NONE',  ( 53.29490495164537833, -11.46446609406722850, -97.50000000000002842 ) ) ;
#9466 = CONICAL_SURFACE ( 'NONE', #7786, 11.96410161513786008, 0.2617993877991461882 ) ;
#9467 = CARTESIAN_POINT ( 'NONE',  ( -15.99999999999999645, 43.00000000000000000, -7.366666666666667140 ) ) ;
#9468 = AXIS2_PLACEMENT_3D ( 'NONE', #7551, #4523, #5353 ) ;
#9469 = DIRECTION ( 'NONE',  ( -1.000000000000000000, 0.000000000000000000, 0.000000000000000000 ) ) ;
#9470 = VECTOR ( 'NONE', #1584, 1000.000000000000000 ) ;
#9471 = LINE ( 'NONE', #2849, #3326 ) ;
#9472 = VECTOR ( 'NONE', #3068, 1000.000000000000000 ) ;
#9473 = VERTEX_POINT ( 'NONE', #3676 ) ;
#9474 = DIRECTION ( 'NONE',  ( 0.000000000000000000, 0.000000000000000000, -1.000000000000000000 ) ) ;
#9475 = NEXT_ASSEMBLY_USAGE_OCCURRENCE ( 'NAUO1', ' ', ' ', #3358, #3945, $ ) ;
#9476 = NEXT_ASSEMBLY_USAGE_OCCURRENCE ( 'NAUO2', ' ', ' ', #3358, #9048, $ ) ;
#9477 = NEXT_ASSEMBLY_USAGE_OCCURRENCE ( 'NAUO3', ' ', ' ', #3358, #3945, $ ) ;
#9478 = NEXT_ASSEMBLY_USAGE_OCCURRENCE ( 'NAUO4', ' ', ' ', #3358, #2939, $ ) ;
#9479 = NEXT_ASSEMBLY_USAGE_OCCURRENCE ( 'NAUO5', ' ', ' ', #3358, #8051, $ ) ;
#9480 = NEXT_ASSEMBLY_USAGE_OCCURRENCE ( 'NAUO6', ' ', ' ', #3358, #6069, $ ) ;
#9481 = NEXT_ASSEMBLY_USAGE_OCCURRENCE ( 'NAUO7', ' ', ' ', #3358, #9048, $ ) ;
#9482 = NEXT_ASSEMBLY_USAGE_OCCURRENCE ( 'NAUO8', ' ', ' ', #3358, #9048, $ ) ;
#9483 = NEXT_ASSEMBLY_USAGE_OCCURRENCE ( 'NAUO9', ' ', ' ', #3358, #9048, $ ) ;
#9484 = NEXT_ASSEMBLY_USAGE_OCCURRENCE ( 'NAUO10', ' ', ' ', #3358, #8051, $ ) ;
#9485 = NEXT_ASSEMBLY_USAGE_OCCURRENCE ( 'NAUO11', ' ', ' ', #3358, #7762, $ ) ;
#9486 = NEXT_ASSEMBLY_USAGE_OCCURRENCE ( 'NAUO12', ' ', ' ', #3358, #2939, $ ) ;
#9487 = NEXT_ASSEMBLY_USAGE_OCCURRENCE ( 'NAUO13', ' ', ' ', #3358, #6069, $ ) ;
#9488 = NEXT_ASSEMBLY_USAGE_OCCURRENCE ( 'NAUO14', ' ', ' ', #3358, #6069, $ ) ;
#9489 = NEXT_ASSEMBLY_USAGE_OCCURRENCE ( 'NAUO15', ' ', ' ', #3358, #6069, $ ) ;
#9490 = NEXT_ASSEMBLY_USAGE_OCCURRENCE ( 'NAUO16', ' ', ' ', #3358, #6069, $ ) ;
#9491 = NEXT_ASSEMBLY_USAGE_OCCURRENCE ( 'NAUO17', ' ', ' ', #3358, #6069, $ ) ;
#9492 = NEXT_ASSEMBLY_USAGE_OCCURRENCE ( 'NAUO18', ' ', ' ', #3358, #6069, $ ) ;
#9493 = NEXT_ASSEMBLY_USAGE_OCCURRENCE ( 'NAUO19', ' ', ' ', #3358, #6069, $ ) ;
#9494 = NEXT_ASSEMBLY_USAGE_OCCURRENCE ( 'NAUO20', ' ', ' ', #3358, #6069, $ ) ;
#9495 = NEXT_ASSEMBLY_USAGE_OCCURRENCE ( 'NAUO21', ' ', ' ', #3358, #6069, $ ) ;
#9496 = NEXT_ASSEMBLY_USAGE_OCCURRENCE ( 'NAUO22', ' ', ' ', #3358, #6069, $ ) ;
#9497 = NEXT_ASSEMBLY_USAGE_OCCURRENCE ( 'NAUO23', ' ', ' ', #3358, #6069, $ ) ;
#9498 = NEXT_ASSEMBLY_USAGE_OCCURRENCE ( 'NAUO24', ' ', ' ', #3358, #6069, $ ) ;
#9499 = NEXT_ASSEMBLY_USAGE_OCCURRENCE ( 'NAUO25', ' ', ' ', #3358, #6069, $ ) ;
#9500 = NEXT_ASSEMBLY_USAGE_OCCURRENCE ( 'NAUO26', ' ', ' ', #3358, #6069, $ ) ;
#9501 = NEXT_ASSEMBLY_USAGE_OCCURRENCE ( 'NAUO27', ' ', ' ', #3358, #6069, $ ) ;
#9502=COLOUR_RGB('Dark Blue',0.08,0.2,0.34);
#9503=FILL_AREA_STYLE_COLOUR('',#9502);
#9504=FILL_AREA_STYLE('',(#9503));
#9505=SURFACE_STYLE_FILL_AREA(#9504);
#9506=SURFACE_SIDE_STYLE('',(#9505));
#9507=SURFACE_STYLE_USAGE(.BOTH.,#9506);
#9508=PRESENTATION_STYLE_ASSIGNMENT((#9507));
#9509=COLOUR_RGB('Light Blue',0.38,0.62,0.78);
#9510=FILL_AREA_STYLE_COLOUR('',#9509);
#9511=FILL_AREA_STYLE('',(#9510));
#9512=SURFACE_STYLE_FILL_AREA(#9511);
#9513=SURFACE_SIDE_STYLE('',(#9512));
#9514=SURFACE_STYLE_USAGE(.BOTH.,#9513);
#9515=PRESENTATION_STYLE_ASSIGNMENT((#9514));
#9516=COLOUR_RGB('Sky Blue',0.24,0.69,0.87);
#9517=FILL_AREA_STYLE_COLOUR('',#9516);
#9518=FILL_AREA_STYLE('',(#9517));
#9519=SURFACE_STYLE_FILL_AREA(#9518);
#9520=SURFACE_SIDE_STYLE('',(#9519));
#9521=SURFACE_STYLE_USAGE(.BOTH.,#9520);
#9522=PRESENTATION_STYLE_ASSIGNMENT((#9521));
#9523=COLOUR_RGB('Grey',0.48,0.52,0.57);
#9524=FILL_AREA_STYLE_COLOUR('',#9523);
#9525=FILL_AREA_STYLE('',(#9524));
#9526=SURFACE_STYLE_FILL_AREA(#9525);
#9527=SURFACE_SIDE_STYLE('',(#9526));
#9528=SURFACE_STYLE_USAGE(.BOTH.,#9527);
#9529=PRESENTATION_STYLE_ASSIGNMENT((#9528));
#9530=COLOUR_RGB('Black',0.12,0.14,0.17);
#9531=FILL_AREA_STYLE_COLOUR('',#9530);
#9532=FILL_AREA_STYLE('',(#9531));
#9533=SURFACE_STYLE_FILL_AREA(#9532);
#9534=SURFACE_SIDE_STYLE('',(#9533));
#9535=SURFACE_STYLE_USAGE(.BOTH.,#9534);
#9536=PRESENTATION_STYLE_ASSIGNMENT((#9535));
#9537=COLOUR_RGB('Off White',0.89,0.88,0.83);
#9538=FILL_AREA_STYLE_COLOUR('',#9537);
#9539=FILL_AREA_STYLE('',(#9538));
#9540=SURFACE_STYLE_FILL_AREA(#9539);
#9541=SURFACE_SIDE_STYLE('',(#9540));
#9542=SURFACE_STYLE_USAGE(.BOTH.,#9541);
#9543=PRESENTATION_STYLE_ASSIGNMENT((#9542));
ENDSEC;
END-ISO-10303-21;
